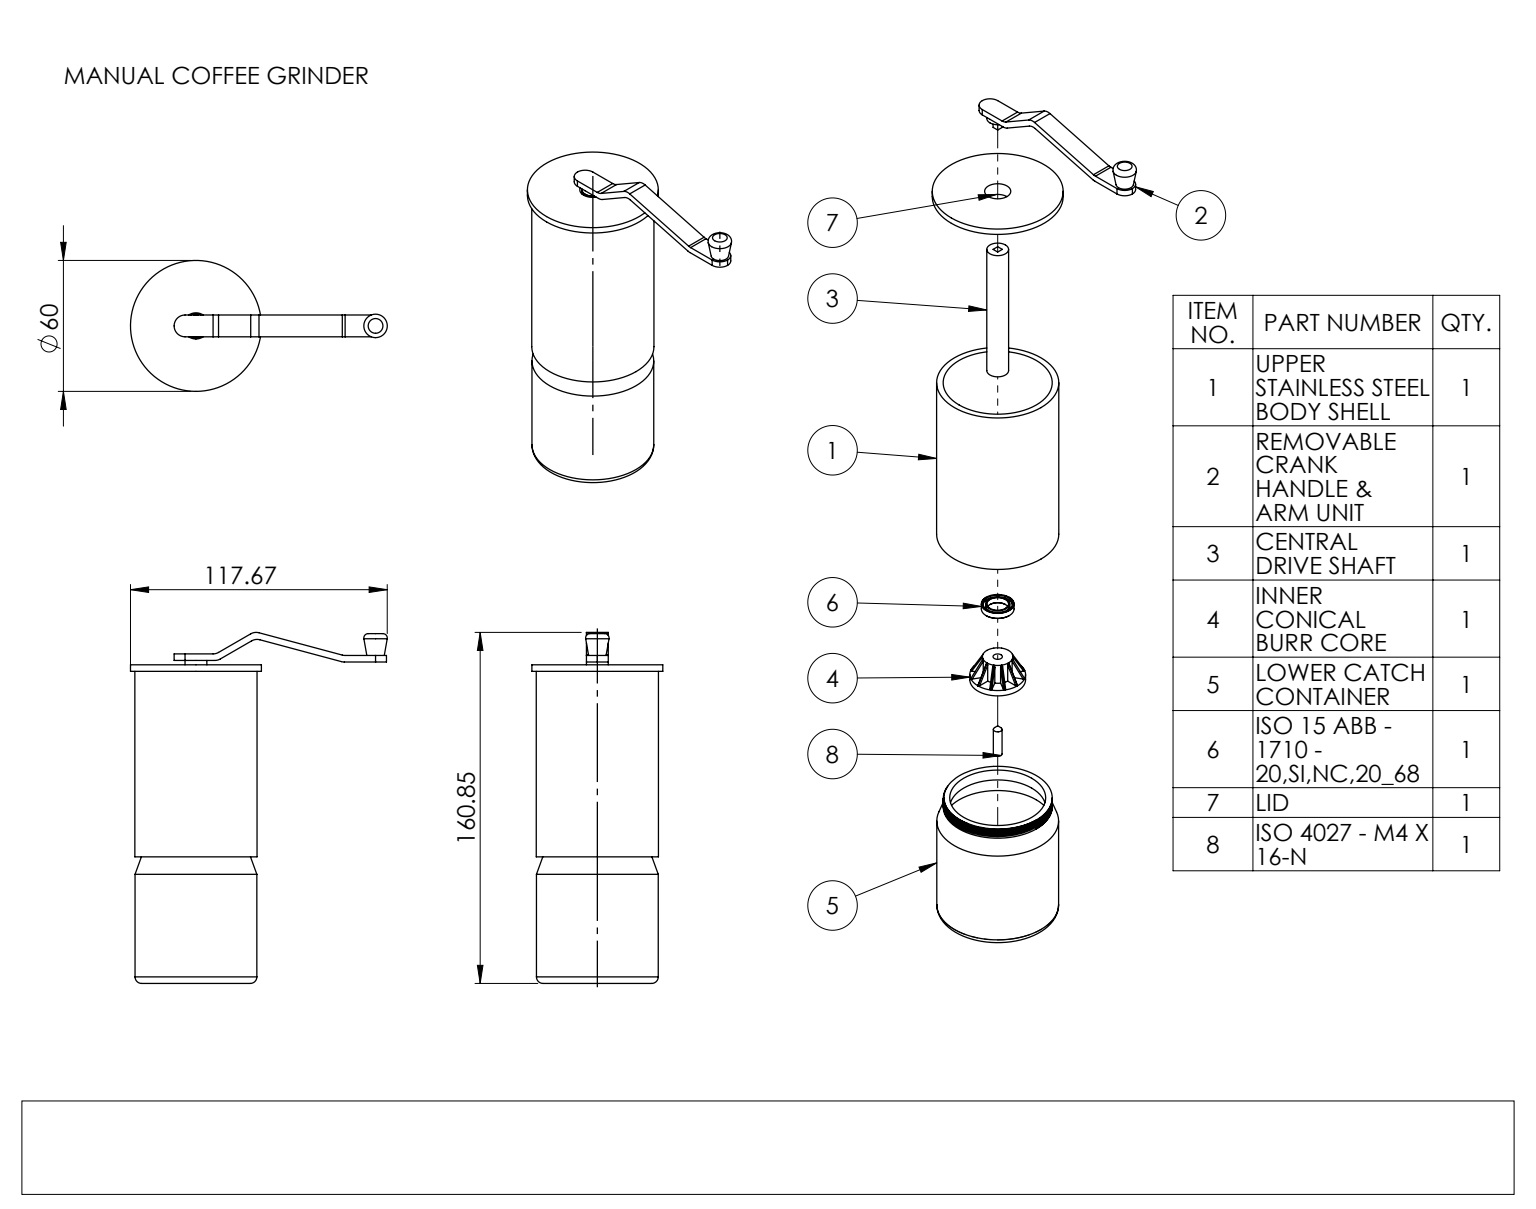
ISO-10303-21;
HEADER;
FILE_DESCRIPTION (('STEP AP214'),
    '1' );
FILE_NAME ('BR-816',
    '2026-10-04T07:23:31',
    ( '' ),
    ( '' ),
    'SwSTEP 2.0',
    'SolidWorks 2026',
    '' );
FILE_SCHEMA (( 'AUTOMOTIVE_DESIGN' ));
ENDSEC;

DATA;
#1 = ORIENTED_EDGE ( 'NONE', *, *, #1320, .F. ) ;
#2 = VERTEX_POINT ( 'NONE', #10191 ) ;
#3 = ORIENTED_EDGE ( 'NONE', *, *, #5333, .F. ) ;
#4 = ORIENTED_EDGE ( 'NONE', *, *, #9160, .T. ) ;
#5 = AXIS2_PLACEMENT_3D ( 'NONE', #6946, #2717, #1088 ) ;
#6 = DIRECTION ( 'NONE',  ( -0.000000000000000000, -1.000000000000000000, -0.000000000000000000 ) ) ;
#7 = CARTESIAN_POINT ( 'NONE',  ( -10.19839929293505776, 0.5312499990440845421, -24.62111388750000174 ) ) ;
#8 = VECTOR ( 'NONE', #4080, 1000.000000000000114 ) ;
#9 = CARTESIAN_POINT ( 'NONE',  ( 1.507608415688466075E-15, 0.6437499990440845865, -24.62111388750000174 ) ) ;
#10 = CARTESIAN_POINT ( 'NONE',  ( 1.530808498934191521E-15, 3.250000000000000444, -25.00000000000000000 ) ) ;
#11 = CARTESIAN_POINT ( 'NONE',  ( -18.60400172474273361, 25.00000000000000000, -7.276923788646512570 ) ) ;
#12 = CARTESIAN_POINT ( 'NONE',  ( 10.00000000000000000, 90.00000000000001421, -5.000000000000000000 ) ) ;
#13 = CARTESIAN_POINT ( 'NONE',  ( 6.296693311223917178, 19.03096903053430822, -3.058047309049999996 ) ) ;
#14 = PRODUCT_DEFINITION ( 'UNKNOWN', '', #3514, #8030 ) ;
#15 = CARTESIAN_POINT ( 'NONE',  ( 24.62111388749999463, 5.156249999044083765, 10.19839929293507730 ) ) ;
#16 = FACE_OUTER_BOUND ( 'NONE', #4981, .T. ) ;
#17 = EDGE_LOOP ( 'NONE', ( #5267, #4224, #10502 ) ) ;
#18 = ORIENTED_EDGE ( 'NONE', *, *, #6824, .T. ) ;
#19 = AXIS2_PLACEMENT_3D ( 'NONE', #2994, #5611, #7166 ) ;
#20 = VERTEX_POINT ( 'NONE', #2725 ) ;
#21 = DIRECTION ( 'NONE',  ( -0.000000000000000000, 1.000000000000000000, -0.000000000000000000 ) ) ;
#22 = EDGE_LOOP ( 'NONE', ( #2895, #8859 ) ) ;
#23 = FACE_OUTER_BOUND ( 'NONE', #10644, .T. ) ;
#24 = CIRCLE ( 'NONE', #8496, 7.500000000000000888 ) ;
#25 = DIRECTION ( 'NONE',  ( 0.000000000000000000, 0.000000000000000000, -1.000000000000000000 ) ) ;
#26 = EDGE_CURVE ( 'NONE', #5713, #6934, #4532, .T. ) ;
#27 = CARTESIAN_POINT ( 'NONE',  ( -1.399999999999998579, 1.126651916477733026E-15, 7.500000000000007994 ) ) ;
#28 = ADVANCED_FACE ( 'NONE', ( #7832 ), #3504, .F. ) ;
#29 =( BOUNDED_CURVE ( )  B_SPLINE_CURVE ( 2, ( #1490, #9059, #4872, #2466, #7337, #5796, #6516, #4977, #5693, #9821, #8329, #10667, #710, #4147, #8268, #1536, #6469, #7289, #10712, #8217, #9874, #10767, #4922, #6628, #4037, #7506, #659, #2414, #7388, #6572, #5852, #9934, #4089, #2367, #5744, #10884, #9103, #7444, #3285, #9986, #9157, #6688, #4816, #10043, #9208, #3929, #1653, #8998, #5036, #8384, #2255, #5638, #1426, #9505, #8609, #7675, #9449, #6799, #7559, #10941, #4194, #1937, #2745, #104, #163, #6090, #1057, #8554, #946, #4431, #10334, #6920, #2627, #4366, #9319, #6026, #8495, #6851, #10273, #882, #2520 ),
 .UNSPECIFIED., .F., .F. ) 
 B_SPLINE_CURVE_WITH_KNOTS ( ( 3, 2, 2, 2, 2, 2, 2, 2, 2, 2, 2, 2, 2, 2, 2, 2, 2, 2, 2, 2, 2, 2, 2, 2, 2, 2, 2, 2, 2, 2, 2, 2, 2, 2, 2, 2, 2, 2, 2, 2, 3 ),
 ( 0.000000000000000000, 0.02500000000000000139, 0.05000000000000000278, 0.07499999999999999722, 0.1000000000000000056, 0.1250000000000000000, 0.1499999999999999944, 0.1749999999999999889, 0.2000000000000000111, 0.2250000000000000056, 0.2500000000000000000, 0.2750000000000000222, 0.2999999999999999889, 0.3250000000000000111, 0.3499999999999999778, 0.3750000000000000000, 0.4000000000000000222, 0.4249999999999999889, 0.4500000000000000111, 0.4749999999999999778, 0.5000000000000000000, 0.5250000000000000222, 0.5500000000000000444, 0.5749999999999999556, 0.5999999999999999778, 0.6250000000000000000, 0.6500000000000000222, 0.6750000000000000444, 0.6999999999999999556, 0.7249999999999999778, 0.7500000000000000000, 0.7750000000000000222, 0.8000000000000000444, 0.8249999999999999556, 0.8499999999999999778, 0.8750000000000000000, 0.9000000000000000222, 0.9250000000000000444, 0.9499999999999999556, 0.9749999999999999778, 1.000000000000000000 ),
 .UNSPECIFIED. ) 
 CURVE ( )  GEOMETRIC_REPRESENTATION_ITEM ( )  RATIONAL_B_SPLINE_CURVE ( ( 1.000000000000000000, 0.9238795325112867385, 1.000000000000000000, 0.9238795325112867385, 1.000000000000000000, 0.9238795325112867385, 1.000000000000000000, 0.9238795325112867385, 1.000000000000000000, 0.9238795325112867385, 1.000000000000000000, 0.9238795325112867385, 1.000000000000000000, 0.9238795325112867385, 1.000000000000000000, 0.9238795325112867385, 1.000000000000000000, 0.9238795325112867385, 1.000000000000000000, 0.9238795325112867385, 1.000000000000000000, 0.9238795325112867385, 1.000000000000000000, 0.9238795325112867385, 1.000000000000000000, 0.9238795325112867385, 1.000000000000000000, 0.9238795325112867385, 1.000000000000000000, 0.9238795325112867385, 1.000000000000000000, 0.9238795325112867385, 1.000000000000000000, 0.9238795325112867385, 1.000000000000000000, 0.9238795325112867385, 1.000000000000000000, 0.9238795325112867385, 1.000000000000000000, 0.9238795325112867385, 1.000000000000000000, 0.9238795325112867385, 1.000000000000000000, 0.9238795325112867385, 1.000000000000000000, 0.9238795325112867385, 1.000000000000000000, 0.9238795325112867385, 1.000000000000000000, 0.9238795325112867385, 1.000000000000000000, 0.9238795325112867385, 1.000000000000000000, 0.9238795325112867385, 1.000000000000000000, 0.9238795325112867385, 1.000000000000000000, 0.9238795325112867385, 1.000000000000000000, 0.9238795325112867385, 1.000000000000000000, 0.9238795325112867385, 1.000000000000000000, 0.9238795325112867385, 1.000000000000000000, 0.9238795325112867385, 1.000000000000000000, 0.9238795325112867385, 1.000000000000000000, 0.9238795325112867385, 1.000000000000000000, 0.9238795325112867385, 1.000000000000000000, 0.9238795325112867385, 1.000000000000000000, 0.9238795325112867385, 1.000000000000000000, 0.9238795325112867385, 1.000000000000000000, 0.9238795325112867385, 1.000000000000000000 ) ) 
 REPRESENTATION_ITEM ( '' )  );
#30 = VECTOR ( 'NONE', #2527, 1000.000000000000000 ) ;
#31 = VECTOR ( 'NONE', #278, 1000.000000000000000 ) ;
#32 = ADVANCED_FACE ( 'NONE', ( #4472 ), #1742, .F. ) ;
#33 = ORIENTED_EDGE ( 'NONE', *, *, #3191, .T. ) ;
#34 = AXIS2_PLACEMENT_3D ( 'NONE', #3449, #3389, #7599 ) ;
#35 = DIRECTION ( 'NONE',  ( 0.000000000000000000, 0.000000000000000000, 1.000000000000000000 ) ) ;
#36 = FACE_OUTER_BOUND ( 'NONE', #8599, .T. ) ;
#37 = PLANE ( 'NONE',  #10541 ) ;
#38 = FACE_OUTER_BOUND ( 'NONE', #4930, .T. ) ;
#39 = VERTEX_POINT ( 'NONE', #260 ) ;
#40 = CIRCLE ( 'NONE', #9387, 2.999999999999999112 ) ;
#41 = LINE ( 'NONE', #2461, #2290 ) ;
#42 = AXIS2_PLACEMENT_3D ( 'NONE', #2337, #7419, #8866 ) ;
#43 = CARTESIAN_POINT ( 'NONE',  ( 0.2251666049839524120, 2.449293598294711838E-16, 2.000000000000004441 ) ) ;
#44 = DIRECTION ( 'NONE',  ( 0.000000000000000000, 0.000000000000000000, -1.000000000000000000 ) ) ;
#45 = EDGE_CURVE ( 'NONE', #4079, #9358, #1978, .T. ) ;
#46 = DIRECTION ( 'NONE',  ( -0.000000000000000000, -1.000000000000000000, -0.000000000000000000 ) ) ;
#47 = ORIENTED_EDGE ( 'NONE', *, *, #865, .T. ) ;
#48 = TOROIDAL_SURFACE ( 'NONE', #9050, 24.91176187412963117, 3.000000000000000000 ) ;
#49 = VECTOR ( 'NONE', #6901, 1000.000000000000000 ) ;
#50 = EDGE_CURVE ( 'NONE', #1424, #5838, #3619, .T. ) ;
#51 = CARTESIAN_POINT ( 'NONE',  ( -10.19839929293507552, 1.081249999044084475, 24.62111388749999463 ) ) ;
#52 = CARTESIAN_POINT ( 'NONE',  ( -10.19839929293505776, 1.706249999044084698, -24.62111388750000174 ) ) ;
#53 = LINE ( 'NONE', #1004, #7949 ) ;
#54 = VECTOR ( 'NONE', #4758, 1000.000000000000000 ) ;
#55 = CARTESIAN_POINT ( 'NONE',  ( 15.13990010960488952, -0.001000000000001000089, -5.276923788646758595 ) ) ;
#56 = CARTESIAN_POINT ( 'NONE',  ( 19.74999999999998934, -0.001000000000001000089, -3.000000000000067946 ) ) ;
#57 = VERTEX_POINT ( 'NONE', #5944 ) ;
#58 = CARTESIAN_POINT ( 'NONE',  ( -2.999999999999998224, 25.00000000000000000, -15.75000000000000355 ) ) ;
#59 = FILL_AREA_STYLE_COLOUR ( '', #6484 ) ;
#60 = CARTESIAN_POINT ( 'NONE',  ( -1.500000000000000444, 83.00000000000000000, -1.500000000000000222 ) ) ;
#61 = CARTESIAN_POINT ( 'NONE',  ( -4.592425496802574367E-15, 2.362499998088169129, 25.00000000000000000 ) ) ;
#62 = DIRECTION ( 'NONE',  ( 0.000000000000000000, 1.000000000000000000, 0.000000000000000000 ) ) ;
#63 = PLANE ( 'NONE',  #9863 ) ;
#64 = VECTOR ( 'NONE', #5356, 1000.000000000000000 ) ;
#65 = ORIENTED_EDGE ( 'NONE', *, *, #1287, .F. ) ;
#66 = EDGE_CURVE ( 'NONE', #3225, #5856, #203, .T. ) ;
#67 = ORIENTED_EDGE ( 'NONE', *, *, #4182, .T. ) ;
#68 = ORIENTED_EDGE ( 'NONE', *, *, #3846, .T. ) ;
#69 = VERTEX_POINT ( 'NONE', #5118 ) ;
#70 = UNCERTAINTY_MEASURE_WITH_UNIT (LENGTH_MEASURE( 1.000000000000000082E-05 ), #3920, 'distance_accuracy_value', 'NONE');
#71 = DIRECTION ( 'NONE',  ( -0.000000000000000000, -1.000000000000000000, -0.000000000000000000 ) ) ;
#72 = CARTESIAN_POINT ( 'NONE',  ( -10.19839929293507552, 0.9062499990440844311, 24.62111388749999463 ) ) ;
#73 = CARTESIAN_POINT ( 'NONE',  ( 7.347880794884120722E-16, 82.00000000000000000, -6.000000000000000888 ) ) ;
#74 = CARTESIAN_POINT ( 'NONE',  ( 24.62111388750000174, 2.393749999044084475, 0.000000000000000000 ) ) ;
#75 = CARTESIAN_POINT ( 'NONE',  ( -25.00000000000000000, 0.4375000000000000000, -10.35533905932738108 ) ) ;
#76 = CARTESIAN_POINT ( 'NONE',  ( 17.10400172474269098, 28.00000000000000000, 9.874999999999957367 ) ) ;
#77 = ORIENTED_EDGE ( 'NONE', *, *, #7857, .F. ) ;
#78 = CARTESIAN_POINT ( 'NONE',  ( 3.785909150703048454, 19.34316356887877220, -5.890223162633865250 ) ) ;
#79 = CARTESIAN_POINT ( 'NONE',  ( 0.000000000000000000, 5.000000000000000000, 0.000000000000000000 ) ) ;
#80 = CARTESIAN_POINT ( 'NONE',  ( -17.67766952966369232, 0.6250000000000000000, 17.67766952966368876 ) ) ;
#81 = CARTESIAN_POINT ( 'NONE',  ( -25.00000000000000000, 3.112499998088169129, -3.061616997868383043E-15 ) ) ;
#82 = ORIENTED_EDGE ( 'NONE', *, *, #3385, .T. ) ;
#83 = ORIENTED_EDGE ( 'NONE', *, *, #9025, .F. ) ;
#84 = ORIENTED_EDGE ( 'NONE', *, *, #2390, .T. ) ;
#85 = PRODUCT_DEFINITION_SHAPE ( 'NONE', 'NONE',  #10954 ) ;
#86 = DIRECTION ( 'NONE',  ( -0.000000000000000000, 1.000000000000000000, 0.000000000000000000 ) ) ;
#87 = FACE_OUTER_BOUND ( 'NONE', #4011, .T. ) ;
#88 = FACE_OUTER_BOUND ( 'NONE', #5727, .T. ) ;
#89 = CARTESIAN_POINT ( 'NONE',  ( 6.999999999999997335, 19.66631150450990617, 0.1668442477450632899 ) ) ;
#90 = FACE_OUTER_BOUND ( 'NONE', #9620, .T. ) ;
#91 = CARTESIAN_POINT ( 'NONE',  ( 1.040834085586084257E-14, 88.00000000000001421, -4.999999999999987566 ) ) ;
#92 = CARTESIAN_POINT ( 'NONE',  ( 12.47307621135333200, 25.00000000000000000, 15.60400172474264835 ) ) ;
#93 = VERTEX_POINT ( 'NONE', #1861 ) ;
#94 = EDGE_CURVE ( 'NONE', #2407, #2818, #6149, .T. ) ;
#95 = DIRECTION ( 'NONE',  ( -0.000000000000000000, -1.000000000000000000, -0.000000000000000000 ) ) ;
#96 = SURFACE_SIDE_STYLE ('',( #6842 ) ) ;
#97 = CARTESIAN_POINT ( 'NONE',  ( 24.99999999999999289, 5.549999998088169129, 10.35533905932739529 ) ) ;
#98 = CARTESIAN_POINT ( 'NONE',  ( 24.62111388750000174, 0.4562499990440845310, -10.19839929293505776 ) ) ;
#99 = ORIENTED_EDGE ( 'NONE', *, *, #3561, .F. ) ;
#100 = LINE ( 'NONE', #5208, #8824 ) ;
#101 = CARTESIAN_POINT ( 'NONE',  ( 17.10400172474269098, 28.00000000000000000, 9.874999999999957367 ) ) ;
#102 = ORIENTED_EDGE ( 'NONE', *, *, #949, .F. ) ;
#103 = CARTESIAN_POINT ( 'NONE',  ( 19.74999999999998934, 25.00000000000000000, -3.000000000000067946 ) ) ;
#104 = CARTESIAN_POINT ( 'NONE',  ( 24.62111388749999108, 4.156249999044084653, 10.19839929293507730 ) ) ;
#105 = ADVANCED_FACE ( 'NONE', ( #143 ), #1537, .T. ) ;
#106 = EDGE_CURVE ( 'NONE', #5745, #5240, #6492, .T. ) ;
#107 = CARTESIAN_POINT ( 'NONE',  ( -4.522825247065398226E-15, 3.143749999044084475, 24.62111388750000174 ) ) ;
#108 = DIRECTION ( 'NONE',  ( 0.000000000000000000, -2.775557561562888270E-17, -1.000000000000000000 ) ) ;
#109 = CARTESIAN_POINT ( 'NONE',  ( -20.63749999999999929, 0.000000000000000000, 0.000000000000000000 ) ) ;
#110 = DIRECTION ( 'NONE',  ( 0.000000000000000000, 0.000000000000000000, 1.000000000000000000 ) ) ;
#111 = ORIENTED_EDGE ( 'NONE', *, *, #6802, .F. ) ;
#112 = CARTESIAN_POINT ( 'NONE',  ( 3.061616997868383043E-15, 27.99999999999999645, 25.00000000000000000 ) ) ;
#113 =( NAMED_UNIT ( * ) SI_UNIT ( $, .STERADIAN. ) SOLID_ANGLE_UNIT ( ) );
#114 = DIRECTION ( 'NONE',  ( 1.000000000000000000, 0.000000000000000000, -0.000000000000000000 ) ) ;
#115 = CARTESIAN_POINT ( 'NONE',  ( 0.000000000000000000, 20.00000000000000355, 0.000000000000000000 ) ) ;
#116 = CARTESIAN_POINT ( 'NONE',  ( -25.00000000000000000, 2.112499998088169129, -3.061616997868383043E-15 ) ) ;
#117 = CARTESIAN_POINT ( 'NONE',  ( 2.449293598294706513E-15, 20.00000000000000355, -20.00000000000000000 ) ) ;
#118 = CARTESIAN_POINT ( 'NONE',  ( 17.67766952966368521, 2.875000000000000000, 17.67766952966369232 ) ) ;
#119 = EDGE_CURVE ( 'NONE', #6443, #1427, #3381, .T. ) ;
#120 = VERTEX_POINT ( 'NONE', #1095 ) ;
#121 = ORIENTED_EDGE ( 'NONE', *, *, #10240, .T. ) ;
#122 = VERTEX_POINT ( 'NONE', #5243 ) ;
#123 = ORIENTED_EDGE ( 'NONE', *, *, #7539, .F. ) ;
#124 = CARTESIAN_POINT ( 'NONE',  ( 0.000000000000000000, 85.00000000000000000, 0.000000000000000000 ) ) ;
#125 = CARTESIAN_POINT ( 'NONE',  ( -10.19839929293507552, 5.081249999044084475, 24.62111388749999463 ) ) ;
#126 = CARTESIAN_POINT ( 'NONE',  ( 17.67766952966369232, 0.7374999980881691286, -17.67766952966369232 ) ) ;
#127 = CARTESIAN_POINT ( 'NONE',  ( 10.19839929293506486, 1.206249999044084698, 24.62111388749999819 ) ) ;
#128 = CARTESIAN_POINT ( 'NONE',  ( -24.62111388750000884, 3.781249999044084653, 10.19839929293505421 ) ) ;
#129 = CARTESIAN_POINT ( 'NONE',  ( -25.00000000000001066, 3.174999998088169573, 10.35533905932737397 ) ) ;
#130 = EDGE_CURVE ( 'NONE', #7410, #4070, #2608, .T. ) ;
#131 = ORIENTED_EDGE ( 'NONE', *, *, #4600, .T. ) ;
#132 = LINE ( 'NONE', #3493, #145 ) ;
#133 = FACE_BOUND ( 'NONE', #4065, .T. ) ;
#134 = DIRECTION ( 'NONE',  ( 0.000000000000000000, 0.000000000000000000, -1.000000000000000000 ) ) ;
#135 = CARTESIAN_POINT ( 'NONE',  ( -25.00000000000000000, 0.4375000000000000000, -10.35533905932738108 ) ) ;
#136 = CARTESIAN_POINT ( 'NONE',  ( -7.211537444790369733, 10.00000000000000355, -6.776463540776874517 ) ) ;
#137 = EDGE_LOOP ( 'NONE', ( #3283, #4277, #3194, #1557 ) ) ;
#138 = CLOSED_SHELL ( 'NONE', ( #5912, #7027, #10918, #9263, #5268, #8033, #4039, #8931, #9209, #7081, #6514, #516, #6002, #10646, #9653, #6197, #4591, #507, #1397, #6646, #1299, #2039, #10092, #4594, #8749, #861, #6693, #7676, #7148, #10570, #5853, #5516, #7088, #717, #5052, #4023, #6869, #3689, #10249, #2799, #5302, #2691, #9344, #9035, #8964, #1267, #437, #3259, #9811, #1259, #7773, #2191, #3472, #3885, #1656, #6813, #3576, #3914, #8252, #9299, #6399, #2209, #4947, #674, #661, #4449, #10399, #4818, #868, #5935, #9573, #7951, #2937, #7004, #2676, #5317, #5105, #3750, #6202, #28, #5672, #1968, #3916, #4465, #4519, #8455, #4226, #4367, #4978, #6266, #8625, #8205, #7818, #6087, #10928, #4909, #2609 ) ) ;
#139 =( BOUNDED_CURVE ( )  B_SPLINE_CURVE ( 2, ( #7817, #6880, #1965, #10238, #251, #129, #4337, #7756, #2653 ),
 .UNSPECIFIED., .F., .F. ) 
 B_SPLINE_CURVE_WITH_KNOTS ( ( 3, 2, 2, 2, 3 ),
 ( 0.4500000000000000111, 0.4749999999999999778, 0.5000000000000000000, 0.5250000000000000222, 0.5500000000000000444 ),
 .UNSPECIFIED. ) 
 CURVE ( )  GEOMETRIC_REPRESENTATION_ITEM ( )  RATIONAL_B_SPLINE_CURVE ( ( 1.000000000000000000, 0.9238795325112867385, 1.000000000000000000, 0.9238795325112867385, 1.000000000000000000, 0.9238795325112867385, 1.000000000000000000, 0.9238795325112867385, 1.000000000000000000 ) ) 
 REPRESENTATION_ITEM ( '' )  );
#140 = ORIENTED_EDGE ( 'NONE', *, *, #5576, .T. ) ;
#141 = ORIENTED_EDGE ( 'NONE', *, *, #3333, .T. ) ;
#142 = ORIENTED_EDGE ( 'NONE', *, *, #10441, .F. ) ;
#143 = FACE_OUTER_BOUND ( 'NONE', #4066, .T. ) ;
#144 = ADVANCED_FACE ( 'NONE', ( #9538 ), #8711, .T. ) ;
#145 = VECTOR ( 'NONE', #2655, 1000.000000000000000 ) ;
#146 = DIRECTION ( 'NONE',  ( -0.000000000000000000, -1.000000000000000000, -0.000000000000000000 ) ) ;
#147 = CARTESIAN_POINT ( 'NONE',  ( -17.10400172474254532, 28.00000000000000000, 9.875000000000202505 ) ) ;
#148 = DIRECTION ( 'NONE',  ( 1.000000000000000000, 0.000000000000000000, 0.000000000000000000 ) ) ;
#149 = FACE_OUTER_BOUND ( 'NONE', #10908, .T. ) ;
#150 = CYLINDRICAL_SURFACE ( 'NONE', #10591, 4.500000000000000888 ) ;
#151 = DIRECTION ( 'NONE',  ( -0.8838834764831844382, -0.3535533905932726206, 0.3061862178478983454 ) ) ;
#152 = CARTESIAN_POINT ( 'NONE',  ( -24.62111388750000174, 3.893749999044084475, -3.015216831376932151E-15 ) ) ;
#153 = AXIS2_PLACEMENT_3D ( 'NONE', #2387, #10130, #10796 ) ;
#154 = CIRCLE ( 'NONE', #1379, 12.77350269189627063 ) ;
#155 = ORIENTED_EDGE ( 'NONE', *, *, #4589, .F. ) ;
#156 = CARTESIAN_POINT ( 'NONE',  ( 24.99999999999999289, 4.937500000000000888, 10.35533905932739529 ) ) ;
#157 = CARTESIAN_POINT ( 'NONE',  ( 17.67766952966368521, 5.487499998088169129, 17.67766952966369232 ) ) ;
#158 = CARTESIAN_POINT ( 'NONE',  ( -24.62111388750000174, 4.831249999044084475, -10.19839929293506131 ) ) ;
#159 = CARTESIAN_POINT ( 'NONE',  ( -6.062177826491028654, 20.00000000000000355, -3.500000000000069722 ) ) ;
#160 = CONTEXT_DEPENDENT_SHAPE_REPRESENTATION ( #10845, #7160 ) ;
#161 = CARTESIAN_POINT ( 'NONE',  ( 0.000000000000000000, 85.00000000000000000, 0.000000000000000000 ) ) ;
#162 = CARTESIAN_POINT ( 'NONE',  ( -3.066987298107830995, 10.00000000000000355, 6.312177826491043753 ) ) ;
#163 = CARTESIAN_POINT ( 'NONE',  ( 24.62111388750000174, 4.218749999044084653, 0.000000000000000000 ) ) ;
#164 = CARTESIAN_POINT ( 'NONE',  ( -10.19839929293505776, 0.7062499990440844755, -24.62111388750000174 ) ) ;
#165 = CARTESIAN_POINT ( 'NONE',  ( 4.500000000000000888, 10.10000000000000497, 0.000000000000000000 ) ) ;
#166 = CARTESIAN_POINT ( 'NONE',  ( -25.00000000000000000, 1.049999998088169129, -10.35533905932738108 ) ) ;
#167 = DIRECTION ( 'NONE',  ( 0.000000000000000000, 2.775557561562888270E-17, 1.000000000000000000 ) ) ;
#168 = ORIENTED_EDGE ( 'NONE', *, *, #8555, .T. ) ;
#169 = DIRECTION ( 'NONE',  ( -0.000000000000000000, 1.000000000000000000, 0.000000000000000000 ) ) ;
#170 = CARTESIAN_POINT ( 'NONE',  ( -17.10400172474254532, 28.00000000000000000, 9.875000000000202505 ) ) ;
#171 =( LENGTH_UNIT ( ) NAMED_UNIT ( * ) SI_UNIT ( .MILLI., .METRE. ) );
#172 = CARTESIAN_POINT ( 'NONE',  ( 10.19839929293505953, 0.4062499990440845421, -24.62111388750000174 ) ) ;
#173 = CARTESIAN_POINT ( 'NONE',  ( 2.632990618166809235E-16, 7.000000000000003553, 2.149999999999999911 ) ) ;
#174 = DIRECTION ( 'NONE',  ( 0.000000000000000000, 0.000000000000000000, 1.000000000000000000 ) ) ;
#175 = CARTESIAN_POINT ( 'NONE',  ( -25.00000000000001421, 3.562500000000000444, 10.35533905932737397 ) ) ;
#176 = PRODUCT_DEFINITION_SHAPE ( 'NONE', 'NONE',  #10948 ) ;
#177 = ADVANCED_FACE ( 'NONE', ( #4290 ), #10361, .F. ) ;
#178 = AXIS2_PLACEMENT_3D ( 'NONE', #3237, #7515, #1602 ) ;
#179 = EDGE_LOOP ( 'NONE', ( #3319, #1358, #7705, #7107 ) ) ;
#180 = CIRCLE ( 'NONE', #5817, 7.500000000000007994 ) ;
#181 = ORIENTED_EDGE ( 'NONE', *, *, #2071, .F. ) ;
#182 = EDGE_CURVE ( 'NONE', #2588, #10522, #9482, .T. ) ;
#183 = LINE ( 'NONE', #1845, #502 ) ;
#184 = CARTESIAN_POINT ( 'NONE',  ( 24.62111388749999463, 4.331249999044085364, 10.19839929293507730 ) ) ;
#185 = DIRECTION ( 'NONE',  ( 0.000000000000000000, -1.000000000000000000, 0.000000000000000000 ) ) ;
#186 = CARTESIAN_POINT ( 'NONE',  ( -10.35533905932737575, 3.924999998088169129, -25.00000000000000000 ) ) ;
#187 = CARTESIAN_POINT ( 'NONE',  ( -17.40975659021752975, 3.593749999044084653, -17.40975659021752975 ) ) ;
#188 = FACE_OUTER_BOUND ( 'NONE', #7003, .T. ) ;
#189 = AXIS2_PLACEMENT_3D ( 'NONE', #10549, #390, #1123 ) ;
#190 = VECTOR ( 'NONE', #6922, 1000.000000000000000 ) ;
#191 = DIRECTION ( 'NONE',  ( 1.000000000000000000, 0.000000000000000000, 0.000000000000000000 ) ) ;
#192 = PLANE ( 'NONE',  #1400 ) ;
#193 = DIRECTION ( 'NONE',  ( 0.000000000000000000, 0.000000000000000000, -1.000000000000000000 ) ) ;
#194 = FACE_OUTER_BOUND ( 'NONE', #6105, .T. ) ;
#195 = CARTESIAN_POINT ( 'NONE',  ( -10.35533905932737575, 1.312500000000000444, -25.00000000000000000 ) ) ;
#196 = EDGE_CURVE ( 'NONE', #620, #978, #10271, .T. ) ;
#197 = CARTESIAN_POINT ( 'NONE',  ( -17.67766952966369232, 3.237499998088169573, 17.67766952966368876 ) ) ;
#198 = ORIENTED_EDGE ( 'NONE', *, *, #7378, .T. ) ;
#199 = ORIENTED_EDGE ( 'NONE', *, *, #10771, .T. ) ;
#200 = ORIENTED_EDGE ( 'NONE', *, *, #382, .F. ) ;
#201 = AXIS2_PLACEMENT_3D ( 'NONE', #9799, #474, #7991 ) ;
#202 = PRESENTATION_LAYER_ASSIGNMENT (  '', '', ( #540 ) ) ;
#203 = LINE ( 'NONE', #6782, #2239 ) ;
#204 = EDGE_CURVE ( 'NONE', #10138, #4764, #1958, .T. ) ;
#205 = DIRECTION ( 'NONE',  ( -0.000000000000000000, 1.000000000000000000, -0.000000000000000000 ) ) ;
#206 = EDGE_LOOP ( 'NONE', ( #9870, #5506, #9937, #2232 ) ) ;
#207 = CYLINDRICAL_SURFACE ( 'NONE', #8878, 5.750000000000006217 ) ;
#208 = CARTESIAN_POINT ( 'NONE',  ( -3.223142256880076948E-15, 28.00000000000000000, -15.75000000000000000 ) ) ;
#209 = DIRECTION ( 'NONE',  ( 0.000000000000000000, 0.000000000000000000, 1.000000000000000000 ) ) ;
#210 = CARTESIAN_POINT ( 'NONE',  ( 7.874999999999916511, 28.00000000000000000, -10.63990010960495702 ) ) ;
#211 = CARTESIAN_POINT ( 'NONE',  ( 1.530808498934191521E-15, 1.250000000000000000, -25.00000000000000000 ) ) ;
#212 = AXIS2_PLACEMENT_3D ( 'NONE', #8810, #4790, #575 ) ;
#213 = ORIENTED_EDGE ( 'NONE', *, *, #10024, .F. ) ;
#214 = ORIENTED_EDGE ( 'NONE', *, *, #10048, .F. ) ;
#215 = DIRECTION ( 'NONE',  ( 0.000000000000000000, 0.000000000000000000, 1.000000000000000000 ) ) ;
#216 = CARTESIAN_POINT ( 'NONE',  ( -10.35533905932739174, 4.299999998088169129, 24.99999999999999289 ) ) ;
#217 = CIRCLE ( 'NONE', #6933, 25.00000000000000000 ) ;
#218 = CARTESIAN_POINT ( 'NONE',  ( 17.40975659021752975, 4.518749999044084475, -17.40975659021752975 ) ) ;
#219 = EDGE_LOOP ( 'NONE', ( #2618, #7161, #8269, #2550 ) ) ;
#220 = CARTESIAN_POINT ( 'NONE',  ( 3.061616997868383043E-15, 0.000000000000000000, 25.00000000000000000 ) ) ;
#221 = CARTESIAN_POINT ( 'NONE',  ( 0.000000000000000000, 7.000000000000003553, 0.000000000000000000 ) ) ;
#222 = DIRECTION ( 'NONE',  ( 0.000000000000000000, 1.000000000000000000, 0.000000000000000000 ) ) ;
#223 = CARTESIAN_POINT ( 'NONE',  ( 0.000000000000000000, 25.00000000000000355, -2.000000000000000000 ) ) ;
#224 = VECTOR ( 'NONE', #10052, 1000.000000000000000 ) ;
#225 = AXIS2_PLACEMENT_3D ( 'NONE', #3856, #484, #9861 ) ;
#226 = ORIENTED_EDGE ( 'NONE', *, *, #6126, .T. ) ;
#227 = CIRCLE ( 'NONE', #6760, 2.000000000000000000 ) ;
#228 = CARTESIAN_POINT ( 'NONE',  ( -24.62111388750000174, 1.831249999044084475, -10.19839929293506131 ) ) ;
#229 = VECTOR ( 'NONE', #2900, 1000.000000000000000 ) ;
#230 = CARTESIAN_POINT ( 'NONE',  ( 24.99999999999999289, 1.937500000000000000, 10.35533905932739529 ) ) ;
#231 = CARTESIAN_POINT ( 'NONE',  ( -4.522825247065398226E-15, 4.968749999044083765, 24.62111388750000174 ) ) ;
#232 = PLANE ( 'NONE',  #3563 ) ;
#233 = ORIENTED_EDGE ( 'NONE', *, *, #10324, .F. ) ;
#234 = CARTESIAN_POINT ( 'NONE',  ( 1.530808498934191521E-15, 0.8624999980881691286, -25.00000000000000000 ) ) ;
#235 = CARTESIAN_POINT ( 'NONE',  ( -17.67766952966368876, 2.375000000000000000, -17.67766952966369232 ) ) ;
#236 = VECTOR ( 'NONE', #2762, 1000.000000000000000 ) ;
#237 = CARTESIAN_POINT ( 'NONE',  ( -24.62111388750000174, 0.6562499990440845421, -10.19839929293506131 ) ) ;
#238 = DIRECTION ( 'NONE',  ( -0.000000000000000000, 1.000000000000000000, -0.000000000000000000 ) ) ;
#239 = VECTOR ( 'NONE', #5384, 1000.000000000000000 ) ;
#240 = AXIS2_PLACEMENT_3D ( 'NONE', #1921, #5301, #7838 ) ;
#241 = VERTEX_POINT ( 'NONE', #8761 ) ;
#242 = ORIENTED_EDGE ( 'NONE', *, *, #1929, .F. ) ;
#243 = CIRCLE ( 'NONE', #1136, 3.379762621896238883 ) ;
#244 = DIRECTION ( 'NONE',  ( 0.000000000000000000, 1.000000000000000000, 0.000000000000000000 ) ) ;
#245 = CARTESIAN_POINT ( 'NONE',  ( 17.40975659021752975, 3.518749999044084920, -17.40975659021752975 ) ) ;
#246 = LINE ( 'NONE', #73, #236 ) ;
#247 = EDGE_CURVE ( 'NONE', #3577, #5793, #9294, .T. ) ;
#248 = CARTESIAN_POINT ( 'NONE',  ( -25.00000000000001421, 3.174999998088169129, 10.35533905932737397 ) ) ;
#249 = CARTESIAN_POINT ( 'NONE',  ( -24.62111388750000174, 2.656249999044085097, -10.19839929293506131 ) ) ;
#250 = EDGE_CURVE ( 'NONE', #1860, #1446, #9645, .T. ) ;
#251 = CARTESIAN_POINT ( 'NONE',  ( -25.00000000000000000, 3.112499998088169129, -3.061616997868383043E-15 ) ) ;
#252 = CYLINDRICAL_SURFACE ( 'NONE', #1418, 25.00000000000000000 ) ;
#253 = AXIS2_PLACEMENT_3D ( 'NONE', #6290, #1159, #5410 ) ;
#254 = CARTESIAN_POINT ( 'NONE',  ( -25.00000000000000000, 1.437500000000000000, -10.35533905932738108 ) ) ;
#255 = CARTESIAN_POINT ( 'NONE',  ( -13.63990010960498367, 28.00000000000000000, -4.874999999999871214 ) ) ;
#256 = EDGE_CURVE ( 'NONE', #8849, #3847, #4015, .T. ) ;
#257 = VERTEX_POINT ( 'NONE', #2223 ) ;
#258 = VECTOR ( 'NONE', #8917, 1000.000000000000114 ) ;
#259 = ORIENTED_EDGE ( 'NONE', *, *, #4096, .F. ) ;
#260 = CARTESIAN_POINT ( 'NONE',  ( 1.530808498934191521E-15, 0.8624999980881691286, -25.00000000000000000 ) ) ;
#261 = EDGE_CURVE ( 'NONE', #5968, #10806, #9690, .T. ) ;
#262 = FACE_OUTER_BOUND ( 'NONE', #1288, .T. ) ;
#263 = DIRECTION ( 'NONE',  ( 0.6546536707079723127, -0.000000000000000000, -0.7559289460184587250 ) ) ;
#264 = DIRECTION ( 'NONE',  ( 0.000000000000000000, 0.000000000000000000, 1.000000000000000000 ) ) ;
#265 = CARTESIAN_POINT ( 'NONE',  ( -1.500000000000000444, 88.00000000000001421, -1.500000000000000222 ) ) ;
#266 = DIRECTION ( 'NONE',  ( 0.000000000000000000, 0.000000000000000000, -1.000000000000000000 ) ) ;
#267 = DIRECTION ( 'NONE',  ( 0.000000000000000000, 0.000000000000000000, -1.000000000000000000 ) ) ;
#268 = EDGE_CURVE ( 'NONE', #2208, #3766, #1396, .T. ) ;
#269 = CARTESIAN_POINT ( 'NONE',  ( -17.40975659021752975, 3.768749999044084475, -17.40975659021752975 ) ) ;
#270 = EDGE_LOOP ( 'NONE', ( #6260, #9302, #1877, #7015, #4822 ) ) ;
#271 = ORIENTED_EDGE ( 'NONE', *, *, #10865, .F. ) ;
#272 = PRODUCT_DEFINITION_SHAPE ( 'NONE', 'NONE',  #10950 ) ;
#273 = CARTESIAN_POINT ( 'NONE',  ( 24.99999999999999289, 2.937500000000000000, 10.35533905932739529 ) ) ;
#274 = CARTESIAN_POINT ( 'NONE',  ( 10.35533905932738286, 1.424999998088169129, 24.99999999999999645 ) ) ;
#275 = CARTESIAN_POINT ( 'NONE',  ( 17.40975659021752975, 3.518749999044084920, -17.40975659021752975 ) ) ;
#276 =( BOUNDED_CURVE ( )  B_SPLINE_CURVE ( 3, ( #9723, #2251, #5583, #2149 ),
 .UNSPECIFIED., .F., .F. ) 
 B_SPLINE_CURVE_WITH_KNOTS ( ( 4, 4 ),
 ( 2.284520705739658375, 2.356010155625179792 ),
 .UNSPECIFIED. ) 
 CURVE ( )  GEOMETRIC_REPRESENTATION_ITEM ( )  RATIONAL_B_SPLINE_CURVE ( ( 1.000000000000000000, 0.9995741502243209453, 0.9995741502243209453, 1.000000000000000000 ) ) 
 REPRESENTATION_ITEM ( '' )  );
#277 = DIRECTION ( 'NONE',  ( -0.2500000000000041078, -0.8660254037844380415, 0.4330127018922181881 ) ) ;
#278 = DIRECTION ( 'NONE',  ( -0.000000000000000000, 1.000000000000000000, -0.000000000000000000 ) ) ;
#279 = ADVANCED_FACE ( 'NONE', ( #7206 ), #1724, .T. ) ;
#280 = DIRECTION ( 'NONE',  ( -0.000000000000000000, 1.000000000000000000, -0.000000000000000000 ) ) ;
#281 = CARTESIAN_POINT ( 'NONE',  ( -0.5000000000000001110, 10.00000000000000355, -6.982120021884469452 ) ) ;
#282 = CARTESIAN_POINT ( 'NONE',  ( 10.19839929293506486, 5.206249999044084475, 24.62111388749999819 ) ) ;
#283 = DIRECTION ( 'NONE',  ( 0.000000000000000000, 0.000000000000000000, 1.000000000000000000 ) ) ;
#284 = CARTESIAN_POINT ( 'NONE',  ( 10.35533905932737930, 3.187500000000000444, -25.00000000000000000 ) ) ;
#285 = CARTESIAN_POINT ( 'NONE',  ( -10.19839929293505776, 0.7062499990440845865, -24.62111388750000174 ) ) ;
#286 = ORIENTED_EDGE ( 'NONE', *, *, #9789, .F. ) ;
#287 = PLANE ( 'NONE',  #10755 ) ;
#288 = CARTESIAN_POINT ( 'NONE',  ( 1.530808498934191521E-15, 2.250000000000000444, -25.00000000000000000 ) ) ;
#289 = CARTESIAN_POINT ( 'NONE',  ( -17.40975659021753330, 0.8437499990440846531, 17.40975659021752975 ) ) ;
#290 = CARTESIAN_POINT ( 'NONE',  ( -10.35533905932739174, 1.299999998088169129, 24.99999999999999289 ) ) ;
#291 = ORIENTED_EDGE ( 'NONE', *, *, #10657, .F. ) ;
#292 = VERTEX_POINT ( 'NONE', #5447 ) ;
#293 = CARTESIAN_POINT ( 'NONE',  ( -24.62111388750000884, 1.956249999044084475, 10.19839929293505421 ) ) ;
#294 = ORIENTED_EDGE ( 'NONE', *, *, #5471, .F. ) ;
#295 = CARTESIAN_POINT ( 'NONE',  ( 2.500000000000000444, -1.000000000000003109, -0.5773502691896260641 ) ) ;
#296 = CARTESIAN_POINT ( 'NONE',  ( -24.62111388750000174, 3.718749999044084653, -3.015216831376932151E-15 ) ) ;
#297 = DIRECTION ( 'NONE',  ( -2.168404344971010347E-16, 0.000000000000000000, -1.000000000000000000 ) ) ;
#298 = CARTESIAN_POINT ( 'NONE',  ( 10.35533905932737930, 2.799999998088169573, -25.00000000000000000 ) ) ;
#299 = CARTESIAN_POINT ( 'NONE',  ( 24.62111388749999463, 4.156249999044083765, 10.19839929293507730 ) ) ;
#300 = CYLINDRICAL_SURFACE ( 'NONE', #10201, 2.999999999999997335 ) ;
#301 = CARTESIAN_POINT ( 'NONE',  ( -5.978755702618581580, 19.66631150450990617, 3.644491357022453748 ) ) ;
#302 = CARTESIAN_POINT ( 'NONE',  ( 0.2500000000000019984, 0.000000000000000000, -0.4330127018922181326 ) ) ;
#303 = CARTESIAN_POINT ( 'NONE',  ( -25.00000000000001421, 4.562500000000000888, 10.35533905932737397 ) ) ;
#304 = CARTESIAN_POINT ( 'NONE',  ( -15.75000000000000000, 25.00000000000000000, 1.681956355172181189E-13 ) ) ;
#305 = ORIENTED_EDGE ( 'NONE', *, *, #6800, .T. ) ;
#306 = ORIENTED_EDGE ( 'NONE', *, *, #2066, .F. ) ;
#307 = EDGE_CURVE ( 'NONE', #620, #1515, #1911, .T. ) ;
#308 = DIRECTION ( 'NONE',  ( 0.000000000000000000, 1.000000000000000000, 0.000000000000000000 ) ) ;
#309 = ADVANCED_FACE ( 'NONE', ( #3677 ), #6334, .F. ) ;
#310 =( GEOMETRIC_REPRESENTATION_CONTEXT ( 3 ) GLOBAL_UNCERTAINTY_ASSIGNED_CONTEXT ( ( #8038 ) ) GLOBAL_UNIT_ASSIGNED_CONTEXT ( ( #3651, #958, #5094 ) ) REPRESENTATION_CONTEXT ( 'NONE', 'WORKASPACE' ) );
#311 = LINE ( 'NONE', #7774, #4484 ) ;
#312 = CARTESIAN_POINT ( 'NONE',  ( 11.42163336986832611, 7.781088913245561400, -7.171633369868279928 ) ) ;
#313 = CARTESIAN_POINT ( 'NONE',  ( 0.000000000000000000, 0.000000000000000000, 0.000000000000000000 ) ) ;
#314 = CARTESIAN_POINT ( 'NONE',  ( -5.000000000000000000, 90.00000000000001421, 0.000000000000000000 ) ) ;
#315 = CYLINDRICAL_SURFACE ( 'NONE', #5866, 2.999999999999997335 ) ;
#316 = CARTESIAN_POINT ( 'NONE',  ( 17.40975659021752975, 3.518749999044084920, -17.40975659021752975 ) ) ;
#317 = EDGE_CURVE ( 'NONE', #3676, #8924, #362, .T. ) ;
#318 = EDGE_CURVE ( 'NONE', #10892, #10861, #6286, .T. ) ;
#319 = EDGE_CURVE ( 'NONE', #5890, #7487, #2988, .T. ) ;
#320 = AXIS2_PLACEMENT_3D ( 'NONE', #10601, #7911, #7226 ) ;
#321 = ORIENTED_EDGE ( 'NONE', *, *, #1197, .F. ) ;
#322 = CLOSED_SHELL ( 'NONE', ( #1450, #3684, #7028, #7525, #4651, #6943, #8474, #5199, #9776, #1972, #3877, #4730, #6668, #9875, #4249, #1226, #5886, #9953, #7341, #5931, #332, #8208, #7321, #2661, #1784, #4660, #4357, #1897, #2839, #1082, #8702 ) ) ;
#323 = EDGE_CURVE ( 'NONE', #8872, #4838, #1231, .T. ) ;
#324 = CARTESIAN_POINT ( 'NONE',  ( -5.812177826491105037, 10.00000000000000355, 3.933012701892163676 ) ) ;
#325 = CARTESIAN_POINT ( 'NONE',  ( -10.19839929293507375, 3.081249999044084920, 24.62111388749999108 ) ) ;
#326 = FACE_OUTER_BOUND ( 'NONE', #1511, .T. ) ;
#327 = CARTESIAN_POINT ( 'NONE',  ( 82.32050807568876394, 92.28203230275514102, 5.000000000000000000 ) ) ;
#328 = AXIS2_PLACEMENT_3D ( 'NONE', #8665, #3636, #7020 ) ;
#329 = CARTESIAN_POINT ( 'NONE',  ( -10.35533905932735621, 5.299999998088170905, 25.00000000000003197 ) ) ;
#330 = APPLICATION_CONTEXT ( 'automotive_design' ) ;
#331 = AXIS2_PLACEMENT_3D ( 'NONE', #9569, #2055, #5387 ) ;
#332 = ADVANCED_FACE ( 'NONE', ( #499 ), #4567, .T. ) ;
#333 = ORIENTED_EDGE ( 'NONE', *, *, #7900, .F. ) ;
#334 =( BOUNDED_CURVE ( )  B_SPLINE_CURVE ( 3, ( #9140, #1571, #4960, #8309 ),
 .UNSPECIFIED., .F., .F. ) 
 B_SPLINE_CURVE_WITH_KNOTS ( ( 4, 4 ),
 ( 2.284520705739657931, 2.356010155625178015 ),
 .UNSPECIFIED. ) 
 CURVE ( )  GEOMETRIC_REPRESENTATION_ITEM ( )  RATIONAL_B_SPLINE_CURVE ( ( 1.000000000000000000, 0.9995741502243209453, 0.9995741502243209453, 1.000000000000000000 ) ) 
 REPRESENTATION_ITEM ( '' )  );
#335 = EDGE_CURVE ( 'NONE', #6402, #2102, #10397, .T. ) ;
#336 = DIRECTION ( 'NONE',  ( 0.000000000000000000, 0.000000000000000000, -1.000000000000000000 ) ) ;
#337 = AXIS2_PLACEMENT_3D ( 'NONE', #6106, #5930, #7751 ) ;
#338 = CARTESIAN_POINT ( 'NONE',  ( -20.27611860449447079, 4.999999999999999112, 14.06603648214180247 ) ) ;
#339 = LINE ( 'NONE', #8784, #5857 ) ;
#340 = ORIENTED_EDGE ( 'NONE', *, *, #4019, .T. ) ;
#341 = CARTESIAN_POINT ( 'NONE',  ( 3.061616997868383043E-15, 5.000000000000000000, 25.00000000000000000 ) ) ;
#342 = DIRECTION ( 'NONE',  ( 1.000000000000000000, 0.000000000000000000, 0.000000000000000000 ) ) ;
#343 = CYLINDRICAL_SURFACE ( 'NONE', #9212, 12.77350269189627063 ) ;
#344 = CARTESIAN_POINT ( 'NONE',  ( -4.522825247065398226E-15, 3.968749999044084209, 24.62111388750000174 ) ) ;
#345 = CARTESIAN_POINT ( 'NONE',  ( 2.999999999999999112, -0.001000000000001000089, 19.75000000000000000 ) ) ;
#346 = VERTEX_POINT ( 'NONE', #9726 ) ;
#347 = PRODUCT_DEFINITION_FORMATION_WITH_SPECIFIED_SOURCE ( 'ANY', '', #361, .NOT_KNOWN. ) ;
#348 = DIRECTION ( 'NONE',  ( 0.000000000000000000, 0.000000000000000000, -1.000000000000000000 ) ) ;
#349 = CARTESIAN_POINT ( 'NONE',  ( -4.522825247065398226E-15, 1.968749999044084653, 24.62111388750000174 ) ) ;
#350 = CARTESIAN_POINT ( 'NONE',  ( -17.40975659021753330, 5.018749999044084475, 17.40975659021752975 ) ) ;
#351 = CARTESIAN_POINT ( 'NONE',  ( 17.67766952966368521, 4.875000000000000000, 17.67766952966369232 ) ) ;
#352 =( LENGTH_UNIT ( ) NAMED_UNIT ( * ) SI_UNIT ( .MILLI., .METRE. ) );
#353 = LINE ( 'NONE', #3726, #6158 ) ;
#354 = CARTESIAN_POINT ( 'NONE',  ( 6.145599950363597408, 19.66631150450990972, -3.355508642977475198 ) ) ;
#355 = DIRECTION ( 'NONE',  ( 0.000000000000000000, 1.000000000000000000, 0.000000000000000000 ) ) ;
#356 = PLANE ( 'NONE',  #3904 ) ;
#357 = VECTOR ( 'NONE', #4991, 1000.000000000000000 ) ;
#358 = CARTESIAN_POINT ( 'NONE',  ( 25.00000000000000000, 2.000000000000000000, 0.000000000000000000 ) ) ;
#359 = ORIENTED_EDGE ( 'NONE', *, *, #8815, .F. ) ;
#360 = ORIENTED_EDGE ( 'NONE', *, *, #10700, .T. ) ;
#361 = PRODUCT ( 'Removable Crank Handle & Arm Unit', 'Removable Crank Handle & Arm Unit', '', ( #7853 ) ) ;
#362 = LINE ( 'NONE', #3732, #5271 ) ;
#363 = AXIS2_PLACEMENT_3D ( 'NONE', #7383, #10762, #7726 ) ;
#364 = VECTOR ( 'NONE', #7348, 1000.000000000000000 ) ;
#365 = DIRECTION ( 'NONE',  ( -0.000000000000000000, -1.000000000000000000, -0.000000000000000000 ) ) ;
#366 = ORIENTED_EDGE ( 'NONE', *, *, #7588, .T. ) ;
#367 = DIRECTION ( 'NONE',  ( -1.000000000000000000, 5.551115123125781913E-15, 0.000000000000000000 ) ) ;
#368 = CARTESIAN_POINT ( 'NONE',  ( 15.60400172474260927, -0.001000000000001000089, -12.47307621135339062 ) ) ;
#369 = FACE_OUTER_BOUND ( 'NONE', #3316, .T. ) ;
#370 = CARTESIAN_POINT ( 'NONE',  ( -4.336808689942017736E-16, 20.00000000000000355, 6.999999999999997335 ) ) ;
#371 = DIRECTION ( 'NONE',  ( 0.000000000000000000, -0.000000000000000000, 1.000000000000000000 ) ) ;
#372 = CIRCLE ( 'NONE', #6199, 2.999999999999999112 ) ;
#373 = AXIS2_PLACEMENT_3D ( 'NONE', #6188, #3894, #6488 ) ;
#374 = ORIENTED_EDGE ( 'NONE', *, *, #8125, .T. ) ;
#375 = VERTEX_POINT ( 'NONE', #4612 ) ;
#376 = CARTESIAN_POINT ( 'NONE',  ( 17.40975659021752620, 4.268749999044084475, 17.40975659021753330 ) ) ;
#377 = EDGE_CURVE ( 'NONE', #6765, #3339, #3870, .T. ) ;
#378 = CARTESIAN_POINT ( 'NONE',  ( -7.171633369868398056, 7.781088913245559624, 11.42163336986824973 ) ) ;
#379 = CARTESIAN_POINT ( 'NONE',  ( 0.000000000000000000, 82.00000000000000000, 25.00000000000000000 ) ) ;
#380 = CYLINDRICAL_SURFACE ( 'NONE', #9214, 2.999999999999997335 ) ;
#381 = DIRECTION ( 'NONE',  ( 0.000000000000000000, 0.000000000000000000, 1.000000000000000000 ) ) ;
#382 = EDGE_CURVE ( 'NONE', #8258, #528, #7233, .T. ) ;
#383 = ORIENTED_EDGE ( 'NONE', *, *, #5717, .F. ) ;
#384 = AXIS2_PLACEMENT_3D ( 'NONE', #4121, #4890, #851 ) ;
#385 = DIRECTION ( 'NONE',  ( -0.000000000000000000, 1.000000000000000000, -0.000000000000000000 ) ) ;
#386 = CARTESIAN_POINT ( 'NONE',  ( -5.796693311223947376, 10.00000000000000355, 3.924072712834399734 ) ) ;
#387 = VERTEX_POINT ( 'NONE', #2812 ) ;
#388 = EDGE_CURVE ( 'NONE', #2139, #10138, #3054, .T. ) ;
#389 = AXIS2_PLACEMENT_3D ( 'NONE', #6634, #9992, #10835 ) ;
#390 = DIRECTION ( 'NONE',  ( 0.000000000000000000, 0.000000000000000000, 1.000000000000000000 ) ) ;
#391 = DIRECTION ( 'NONE',  ( 0.000000000000000000, 0.000000000000000000, 1.000000000000000000 ) ) ;
#392 = CARTESIAN_POINT ( 'NONE',  ( 15.60400172474269453, 25.00000000000000000, 12.47307621135327693 ) ) ;
#393 = ORIENTED_EDGE ( 'NONE', *, *, #10575, .T. ) ;
#394 = CARTESIAN_POINT ( 'NONE',  ( 24.62111388749999108, 2.156249999044084653, 10.19839929293507730 ) ) ;
#395 = LINE ( 'NONE', #6422, #1735 ) ;
#396 = EDGE_CURVE ( 'NONE', #5862, #7391, #2207, .T. ) ;
#397 = CIRCLE ( 'NONE', #8311, 6.999999999999997335 ) ;
#398 = EDGE_CURVE ( 'NONE', #963, #2292, #395, .T. ) ;
#399 = VERTEX_POINT ( 'NONE', #8842 ) ;
#400 = EDGE_LOOP ( 'NONE', ( #8892, #7575 ) ) ;
#401 = CIRCLE ( 'NONE', #10807, 6.999999999999997335 ) ;
#402 = CIRCLE ( 'NONE', #9394, 2.999999999999999112 ) ;
#403 = CARTESIAN_POINT ( 'NONE',  ( 0.000000000000000000, 20.00000000000000355, -6.999999999999997335 ) ) ;
#404 = CARTESIAN_POINT ( 'NONE',  ( -17.40975659021752975, 2.593749999044084653, -17.40975659021752975 ) ) ;
#405 = CIRCLE ( 'NONE', #9386, 2.000000000000000000 ) ;
#406 = CARTESIAN_POINT ( 'NONE',  ( 24.62111388750000174, 2.393749999044084475, 0.000000000000000000 ) ) ;
#407 = CARTESIAN_POINT ( 'NONE',  ( -25.00000000000000000, 3.437500000000000000, -10.35533905932738108 ) ) ;
#408 = FILL_AREA_STYLE ('',( #5487 ) ) ;
#409 = CIRCLE ( 'NONE', #8520, 0.1000000000000002554 ) ;
#410 = CARTESIAN_POINT ( 'NONE',  ( -17.67766952966368876, 0.9874999980881691286, -17.67766952966369232 ) ) ;
#411 = FACE_OUTER_BOUND ( 'NONE', #2991, .T. ) ;
#412 = AXIS2_PLACEMENT_3D ( 'NONE', #4846, #684, #4789 ) ;
#413 = DIRECTION ( 'NONE',  ( 1.000000000000000000, 0.000000000000000000, 0.000000000000000000 ) ) ;
#414 = EDGE_CURVE ( 'NONE', #5784, #652, #8731, .T. ) ;
#415 = CIRCLE ( 'NONE', #5701, 0.1000000000000002554 ) ;
#416 = VERTEX_POINT ( 'NONE', #5429 ) ;
#417 = VERTEX_POINT ( 'NONE', #2913 ) ;
#418 = ORIENTED_EDGE ( 'NONE', *, *, #7281, .F. ) ;
#419 = ORIENTED_EDGE ( 'NONE', *, *, #8806, .F. ) ;
#420 = CIRCLE ( 'NONE', #2878, 6.750000000000007994 ) ;
#421 = CARTESIAN_POINT ( 'NONE',  ( -25.00000000000001066, 0.5625000000000002220, 10.35533905932737397 ) ) ;
#422 = CARTESIAN_POINT ( 'NONE',  ( 1.499999999999999556, 83.00000000000000000, -1.500000000000000222 ) ) ;
#423 = CARTESIAN_POINT ( 'NONE',  ( -2.857142857142858983, 10.00000000000000355, -9.474358296526935064 ) ) ;
#424 = FACE_OUTER_BOUND ( 'NONE', #721, .T. ) ;
#425 = FACE_OUTER_BOUND ( 'NONE', #10415, .T. ) ;
#426 = PLANE ( 'NONE',  #3198 ) ;
#427 = CIRCLE ( 'NONE', #1301, 5.525000000000006573 ) ;
#428 = EDGE_LOOP ( 'NONE', ( #6689, #3315, #4054 ) ) ;
#429 = ORIENTED_EDGE ( 'NONE', *, *, #6271, .F. ) ;
#430 = ORIENTED_EDGE ( 'NONE', *, *, #4396, .T. ) ;
#431 = CARTESIAN_POINT ( 'NONE',  ( 1.400000000000001910, -1.415534356397074737E-16, -5.100000000000006750 ) ) ;
#432 = DIRECTION ( 'NONE',  ( -0.4999999999999919509, 0.000000000000000000, -0.8660254037844432595 ) ) ;
#433 = DIRECTION ( 'NONE',  ( 1.000000000000000000, 0.000000000000000000, 0.000000000000000000 ) ) ;
#434 = DIRECTION ( 'NONE',  ( 0.000000000000000000, -1.000000000000000000, 0.000000000000000000 ) ) ;
#435 = DIRECTION ( 'NONE',  ( 0.000000000000000000, 0.000000000000000000, 1.000000000000000000 ) ) ;
#436 = EDGE_CURVE ( 'NONE', #1816, #8189, #1374, .T. ) ;
#437 = ADVANCED_FACE ( 'NONE', ( #450 ), #10554, .F. ) ;
#438 = ORIENTED_EDGE ( 'NONE', *, *, #10019, .T. ) ;
#439 = EDGE_CURVE ( 'NONE', #3209, #9663, #8791, .T. ) ;
#440 = LINE ( 'NONE', #3807, #6013 ) ;
#441 = CARTESIAN_POINT ( 'NONE',  ( -4.592425496802574367E-15, 5.362499998088169129, 25.00000000000000000 ) ) ;
#442 = CARTESIAN_POINT ( 'NONE',  ( 1.507608415688466075E-15, 2.643749999044084920, -24.62111388750000174 ) ) ;
#443 = EDGE_LOOP ( 'NONE', ( #4090, #2708 ) ) ;
#444 = CARTESIAN_POINT ( 'NONE',  ( 24.62111388750000174, 5.218749999044084653, 0.000000000000000000 ) ) ;
#445 =( NAMED_UNIT ( * ) SI_UNIT ( $, .STERADIAN. ) SOLID_ANGLE_UNIT ( ) );
#446 = EDGE_CURVE ( 'NONE', #7282, #1433, #4666, .T. ) ;
#447 = CARTESIAN_POINT ( 'NONE',  ( 0.000000000000000000, 20.00000000000000355, 0.000000000000000000 ) ) ;
#448 = VERTEX_POINT ( 'NONE', #1591 ) ;
#449 = CARTESIAN_POINT ( 'NONE',  ( 24.62111388750000174, 4.281249999044084653, -10.19839929293505776 ) ) ;
#450 = FACE_OUTER_BOUND ( 'NONE', #4386, .T. ) ;
#451 = PRODUCT ( 'Upper Stainless Steel Body Shell', 'Upper Stainless Steel Body Shell', '', ( #5141 ) ) ;
#452 = ORIENTED_EDGE ( 'NONE', *, *, #7524, .T. ) ;
#453 = EDGE_CURVE ( 'NONE', #3864, #1133, #3229, .T. ) ;
#454 = CARTESIAN_POINT ( 'NONE',  ( 0.000000000000000000, 88.00000000000001421, 0.000000000000000000 ) ) ;
#455 = CARTESIAN_POINT ( 'NONE',  ( 1.507608415688466075E-15, 4.468749999044084653, -24.62111388750000174 ) ) ;
#456 = CARTESIAN_POINT ( 'NONE',  ( -17.40975659021752975, 1.768749999044084475, -17.40975659021752975 ) ) ;
#457 = VERTEX_POINT ( 'NONE', #3077 ) ;
#458 = CARTESIAN_POINT ( 'NONE',  ( -25.00000000000000000, 1.437500000000000000, -10.35533905932738108 ) ) ;
#459 = EDGE_CURVE ( 'NONE', #2069, #3931, #29, .T. ) ;
#460 = CARTESIAN_POINT ( 'NONE',  ( 0.000000000000000000, 88.00000000000001421, -4.999999999999997335 ) ) ;
#461 = DIRECTION ( 'NONE',  ( 0.000000000000000000, -0.000000000000000000, 1.000000000000000000 ) ) ;
#462 = PLANE ( 'NONE',  #6027 ) ;
#463 = CARTESIAN_POINT ( 'NONE',  ( 17.67766952966369232, 3.737499998088169573, -17.67766952966369232 ) ) ;
#464 = ORIENTED_EDGE ( 'NONE', *, *, #335, .T. ) ;
#465 = ORIENTED_EDGE ( 'NONE', *, *, #1592, .F. ) ;
#466 = CARTESIAN_POINT ( 'NONE',  ( -25.00000000000000000, 0.5000000000000000000, -3.061616997868383043E-15 ) ) ;
#467 = ADVANCED_FACE ( 'NONE', ( #4314 ), #3524, .F. ) ;
#468 = CARTESIAN_POINT ( 'NONE',  ( 2.500000000000000444, 1.000000000000002220, -0.5773502691896270633 ) ) ;
#469 = EDGE_CURVE ( 'NONE', #8735, #3294, #3407, .T. ) ;
#470 = CARTESIAN_POINT ( 'NONE',  ( -5.000000000000000000, 93.00000000000001421, 0.000000000000000000 ) ) ;
#471 = EDGE_LOOP ( 'NONE', ( #8532, #9181, #9575, #7189, #4997, #4095, #6051, #9424 ) ) ;
#472 = CARTESIAN_POINT ( 'NONE',  ( 0.000000000000000000, 20.00000000000000355, 0.000000000000000000 ) ) ;
#473 = CARTESIAN_POINT ( 'NONE',  ( -6.348076211353412823, 10.00000000000000355, 11.26313972081436532 ) ) ;
#474 = DIRECTION ( 'NONE',  ( 0.000000000000000000, 1.000000000000000000, 0.000000000000000000 ) ) ;
#475 = DIRECTION ( 'NONE',  ( 0.000000000000000000, 0.000000000000000000, 1.000000000000000000 ) ) ;
#476 = ORIENTED_EDGE ( 'NONE', *, *, #10844, .F. ) ;
#477 = ORIENTED_EDGE ( 'NONE', *, *, #2129, .T. ) ;
#478 = EDGE_CURVE ( 'NONE', #10364, #8941, #3461, .T. ) ;
#479 = MECHANICAL_DESIGN_GEOMETRIC_PRESENTATION_REPRESENTATION (  '', ( #10362 ), #8224 ) ;
#480 = CARTESIAN_POINT ( 'NONE',  ( -19.39162934935757931, 5.000000000000000888, 15.17115553405142947 ) ) ;
#481 = DIRECTION ( 'NONE',  ( 0.000000000000000000, 0.000000000000000000, -1.000000000000000000 ) ) ;
#482 = CARTESIAN_POINT ( 'NONE',  ( 2.500000000000000444, -1.000000000000003331, 0.5773502691896272854 ) ) ;
#483 = DIRECTION ( 'NONE',  ( 0.000000000000000000, 1.000000000000000000, 0.000000000000000000 ) ) ;
#484 = DIRECTION ( 'NONE',  ( -0.8660254037844451469, 0.000000000000000000, -0.4999999999999887312 ) ) ;
#485 = MECHANICAL_DESIGN_GEOMETRIC_PRESENTATION_REPRESENTATION (  '', ( #10900 ), #6489 ) ;
#486 = VECTOR ( 'NONE', #920, 1000.000000000000000 ) ;
#487 = ORIENTED_EDGE ( 'NONE', *, *, #845, .F. ) ;
#488 = ORIENTED_EDGE ( 'NONE', *, *, #2343, .T. ) ;
#489 = CARTESIAN_POINT ( 'NONE',  ( 19.75000000000001066, 28.00000000000000000, 2.999999999999927613 ) ) ;
#490 = CARTESIAN_POINT ( 'NONE',  ( 1.040834085586084257E-14, 90.00000000000001421, 5.000000000000000000 ) ) ;
#491 = CARTESIAN_POINT ( 'NONE',  ( -1.500000000000000444, 88.00000000000001421, 1.499999999999999778 ) ) ;
#492 = VERTEX_POINT ( 'NONE', #223 ) ;
#493 = DIRECTION ( 'NONE',  ( -0.000000000000000000, -1.000000000000000000, -0.000000000000000000 ) ) ;
#494 = PRESENTATION_STYLE_ASSIGNMENT (( #8112 ) ) ;
#495 = CARTESIAN_POINT ( 'NONE',  ( -12.69999999999998153, 0.000000000000000000, 0.000000000000000000 ) ) ;
#496 = ORIENTED_EDGE ( 'NONE', *, *, #2584, .T. ) ;
#497 = AXIS2_PLACEMENT_3D ( 'NONE', #5910, #6978, #9384 ) ;
#498 = CARTESIAN_POINT ( 'NONE',  ( 1.507608415688466075E-15, 1.468749999044084431, -24.62111388750000174 ) ) ;
#499 = FACE_OUTER_BOUND ( 'NONE', #9815, .T. ) ;
#500 = VERTEX_POINT ( 'NONE', #5316 ) ;
#501 = ORIENTED_EDGE ( 'NONE', *, *, #4410, .F. ) ;
#502 = VECTOR ( 'NONE', #9281, 999.9999999999998863 ) ;
#503 = CARTESIAN_POINT ( 'NONE',  ( 1.507608415688466075E-15, 2.468749999044085097, -24.62111388750000174 ) ) ;
#504 = CARTESIAN_POINT ( 'NONE',  ( 24.62111388749999463, 2.331249999044084031, 10.19839929293507730 ) ) ;
#505 = ORIENTED_EDGE ( 'NONE', *, *, #6617, .F. ) ;
#506 = CARTESIAN_POINT ( 'NONE',  ( 25.00000000000000000, 4.062500000000000000, -10.35533905932737753 ) ) ;
#507 = ADVANCED_FACE ( 'NONE', ( #3586 ), #10212, .F. ) ;
#508 = EDGE_CURVE ( 'NONE', #3100, #1857, #9259, .T. ) ;
#509 = DIRECTION ( 'NONE',  ( -0.000000000000000000, -1.000000000000000000, -0.000000000000000000 ) ) ;
#510 = CARTESIAN_POINT ( 'NONE',  ( 25.00000000000000000, 0.6749999980881690176, -10.35533905932737753 ) ) ;
#511 = DIRECTION ( 'NONE',  ( 0.000000000000000000, 0.000000000000000000, 1.000000000000000000 ) ) ;
#512 = LINE ( 'NONE', #7202, #5833 ) ;
#513 = ORIENTED_EDGE ( 'NONE', *, *, #1407, .T. ) ;
#514 = VERTEX_POINT ( 'NONE', #5086 ) ;
#515 = ORIENTED_EDGE ( 'NONE', *, *, #3176, .F. ) ;
#516 = ADVANCED_FACE ( 'NONE', ( #8437 ), #4251, .F. ) ;
#517 = CARTESIAN_POINT ( 'NONE',  ( 1.399999999999998579, 0.000000000000000000, 0.000000000000000000 ) ) ;
#518 = LINE ( 'NONE', #3202, #8425 ) ;
#519 = DIRECTION ( 'NONE',  ( 0.000000000000000000, 1.502202555303639631E-16, 1.000000000000000000 ) ) ;
#520 = EDGE_CURVE ( 'NONE', #5481, #3253, #2570, .T. ) ;
#521 = CARTESIAN_POINT ( 'NONE',  ( -5.000000000000000000, 93.00000000000001421, 5.000000000000000000 ) ) ;
#522 = DIRECTION ( 'NONE',  ( -0.000000000000000000, 1.000000000000000000, -0.000000000000000000 ) ) ;
#523 = CARTESIAN_POINT ( 'NONE',  ( 5.446152422706636465, 10.00000000000000355, -2.566987298107767490 ) ) ;
#524 = ORIENTED_EDGE ( 'NONE', *, *, #1672, .T. ) ;
#525 = EDGE_CURVE ( 'NONE', #5936, #10248, #7856, .T. ) ;
#526 = CIRCLE ( 'NONE', #1771, 12.77350269189627063 ) ;
#527 = CIRCLE ( 'NONE', #8986, 2.999999999999998668 ) ;
#528 = VERTEX_POINT ( 'NONE', #281 ) ;
#529 = DIRECTION ( 'NONE',  ( 0.000000000000000000, 0.000000000000000000, -1.000000000000000000 ) ) ;
#530 = DIRECTION ( 'NONE',  ( -0.000000000000000000, 1.000000000000000000, -0.000000000000000000 ) ) ;
#531 = LINE ( 'NONE', #8048, #2356 ) ;
#532 = VECTOR ( 'NONE', #6272, 1000.000000000000227 ) ;
#533 = EDGE_CURVE ( 'NONE', #8829, #4450, #8962, .T. ) ;
#534 = VECTOR ( 'NONE', #1707, 1000.000000000000000 ) ;
#535 = CARTESIAN_POINT ( 'NONE',  ( 1.040834085586084257E-14, 90.00000000000001421, 0.000000000000000000 ) ) ;
#536 = DIRECTION ( 'NONE',  ( 0.000000000000000000, 1.000000000000000000, 0.000000000000000000 ) ) ;
#537 = ORIENTED_EDGE ( 'NONE', *, *, #3535, .F. ) ;
#538 = EDGE_LOOP ( 'NONE', ( #10942, #1687, #7523, #476 ) ) ;
#539 = VECTOR ( 'NONE', #2027, 1000.000000000000000 ) ;
#540 = STYLED_ITEM ( 'NONE', ( #5737 ), #3340 ) ;
#541 = FILL_AREA_STYLE_COLOUR ( '', #3347 ) ;
#542 = CARTESIAN_POINT ( 'NONE',  ( 3.061616997868383043E-15, 85.00000000000000000, -25.00000000000000000 ) ) ;
#543 = CARTESIAN_POINT ( 'NONE',  ( 10.19839929293505953, 3.581249999044085364, -24.62111388750000174 ) ) ;
#544 = VERTEX_POINT ( 'NONE', #8636 ) ;
#545 = CARTESIAN_POINT ( 'NONE',  ( 19.75000000000000000, -0.001000000000001000089, -7.291468677852036884E-14 ) ) ;
#546 = CARTESIAN_POINT ( 'NONE',  ( -1.500000000000000444, 83.00000000000000000, 1.499999999999999778 ) ) ;
#547 = CARTESIAN_POINT ( 'NONE',  ( 24.62111388750000174, 1.281249999044084653, -10.19839929293505776 ) ) ;
#548 = DIRECTION ( 'NONE',  ( -0.000000000000000000, 1.000000000000000000, -0.000000000000000000 ) ) ;
#549 = ORIENTED_EDGE ( 'NONE', *, *, #6741, .T. ) ;
#550 = ORIENTED_EDGE ( 'NONE', *, *, #3080, .T. ) ;
#551 = VECTOR ( 'NONE', #10567, 1000.000000000000000 ) ;
#552 = CARTESIAN_POINT ( 'NONE',  ( -25.00000000000001421, 3.174999998088169129, 10.35533905932737397 ) ) ;
#553 = DIRECTION ( 'NONE',  ( 1.000000000000000000, 0.000000000000000000, 0.000000000000000000 ) ) ;
#554 = CARTESIAN_POINT ( 'NONE',  ( -24.62111388750000174, 3.893749999044084475, -3.015216831376932151E-15 ) ) ;
#555 = CARTESIAN_POINT ( 'NONE',  ( -4.592425496802574367E-15, 4.750000000000000000, 25.00000000000000000 ) ) ;
#556 = VECTOR ( 'NONE', #169, 1000.000000000000000 ) ;
#557 = CARTESIAN_POINT ( 'NONE',  ( -6.999999999999994671, 19.66631150450992749, -0.1668442477451158867 ) ) ;
#558 = CARTESIAN_POINT ( 'NONE',  ( -13.63990010960481492, 28.00000000000000000, 7.875000000000163425 ) ) ;
#559 = DIRECTION ( 'NONE',  ( 1.445602896647339163E-16, 0.000000000000000000, 1.000000000000000000 ) ) ;
#560 = DIRECTION ( 'NONE',  ( 0.000000000000000000, 0.000000000000000000, -1.000000000000000000 ) ) ;
#561 = VECTOR ( 'NONE', #1063, 1000.000000000000000 ) ;
#562 = ORIENTED_EDGE ( 'NONE', *, *, #9891, .F. ) ;
#563 = ORIENTED_EDGE ( 'NONE', *, *, #319, .T. ) ;
#564 = VERTEX_POINT ( 'NONE', #7642 ) ;
#565 = AXIS2_PLACEMENT_3D ( 'NONE', #8099, #5732, #433 ) ;
#566 = AXIS2_PLACEMENT_3D ( 'NONE', #6788, #151, #987 ) ;
#567 = EDGE_CURVE ( 'NONE', #9293, #10413, #10782, .T. ) ;
#568 = CARTESIAN_POINT ( 'NONE',  ( 25.00000000000000000, 4.000000000000000000, 0.000000000000000000 ) ) ;
#569 = AXIS2_PLACEMENT_3D ( 'NONE', #4292, #5896, #6784 ) ;
#570 = DIRECTION ( 'NONE',  ( -1.000000000000000000, 0.000000000000000000, 0.000000000000000000 ) ) ;
#571 =( NAMED_UNIT ( * ) PLANE_ANGLE_UNIT ( ) SI_UNIT ( $, .RADIAN. ) );
#572 = AXIS2_PLACEMENT_3D ( 'NONE', #5272, #10857, #4120 ) ;
#573 = CARTESIAN_POINT ( 'NONE',  ( 3.058047309050023088, 10.00000000000000355, -6.296693311223907408 ) ) ;
#574 = EDGE_CURVE ( 'NONE', #8829, #3039, #9473, .T. ) ;
#575 = DIRECTION ( 'NONE',  ( 0.000000000000000000, 0.000000000000000000, -1.000000000000000000 ) ) ;
#576 = AXIS2_PLACEMENT_3D ( 'NONE', #6748, #5973, #10110 ) ;
#577 = CARTESIAN_POINT ( 'NONE',  ( -15.60400172474251690, 28.00000000000000000, 12.47307621135349720 ) ) ;
#578 = CARTESIAN_POINT ( 'NONE',  ( 1.500000000000001332, -2.053912595556539452E-16, -7.400000000000007461 ) ) ;
#579 = ORIENTED_EDGE ( 'NONE', *, *, #4051, .T. ) ;
#580 = ORIENTED_EDGE ( 'NONE', *, *, #5350, .F. ) ;
#581 = AXIS2_PLACEMENT_3D ( 'NONE', #6035, #5977, #10168 ) ;
#582 = EDGE_LOOP ( 'NONE', ( #4342, #8954, #2146, #5276, #930 ) ) ;
#583 = CIRCLE ( 'NONE', #4834, 6.999999999999997335 ) ;
#584 = ORIENTED_EDGE ( 'NONE', *, *, #5586, .F. ) ;
#585 = EDGE_CURVE ( 'NONE', #6763, #4029, #1905, .T. ) ;
#586 = ORIENTED_EDGE ( 'NONE', *, *, #567, .T. ) ;
#587 = AXIS2_PLACEMENT_3D ( 'NONE', #4145, #5850, #2623 ) ;
#588 = DIRECTION ( 'NONE',  ( -1.000000000000000000, 0.000000000000000000, -1.047444401652940007E-14 ) ) ;
#589 = CIRCLE ( 'NONE', #3780, 22.00000000000000355 ) ;
#590 = DIRECTION ( 'NONE',  ( -1.000000000000000000, 0.000000000000000000, 0.000000000000000000 ) ) ;
#591 = EDGE_CURVE ( 'NONE', #811, #698, #1969, .T. ) ;
#592 = PLANE ( 'NONE',  #2028 ) ;
#593 = DIRECTION ( 'NONE',  ( -0.000000000000000000, -1.000000000000000000, -0.000000000000000000 ) ) ;
#594 = DIRECTION ( 'NONE',  ( 0.000000000000000000, 1.000000000000000000, 0.000000000000000000 ) ) ;
#595 = AXIS2_PLACEMENT_3D ( 'NONE', #2399, #9367, #7543 ) ;
#596 = ORIENTED_EDGE ( 'NONE', *, *, #10438, .T. ) ;
#597 = ORIENTED_EDGE ( 'NONE', *, *, #2649, .F. ) ;
#598 = LINE ( 'NONE', #3011, #2601 ) ;
#599 =( NAMED_UNIT ( * ) PLANE_ANGLE_UNIT ( ) SI_UNIT ( $, .RADIAN. ) );
#600 = CARTESIAN_POINT ( 'NONE',  ( -3.924072712834378862, 19.03096903053431888, -5.796693311223959810 ) ) ;
#601 = CARTESIAN_POINT ( 'NONE',  ( -24.62111388750000884, 2.956249999044084475, 10.19839929293505421 ) ) ;
#602 = ADVANCED_FACE ( 'NONE', ( #6052 ), #6853, .T. ) ;
#603 = ORIENTED_EDGE ( 'NONE', *, *, #8062, .F. ) ;
#604 = LINE ( 'NONE', #4915, #6711 ) ;
#605 = DIRECTION ( 'NONE',  ( 0.000000000000000000, 0.000000000000000000, 1.000000000000000000 ) ) ;
#606 = LINE ( 'NONE', #10829, #1633 ) ;
#607 = EDGE_LOOP ( 'NONE', ( #9268, #5348, #7147, #5082, #6374 ) ) ;
#608 = ORIENTED_EDGE ( 'NONE', *, *, #5350, .T. ) ;
#609 = CARTESIAN_POINT ( 'NONE',  ( -25.00000000000000000, 5.112499998088170017, -3.061616997868383043E-15 ) ) ;
#610 = CARTESIAN_POINT ( 'NONE',  ( -20.63749999999999929, 0.000000000000000000, 0.000000000000000000 ) ) ;
#611 = CARTESIAN_POINT ( 'NONE',  ( 24.62111388750000174, 5.393749999044085364, 0.000000000000000000 ) ) ;
#612 = EDGE_LOOP ( 'NONE', ( #729, #7297, #168, #8289 ) ) ;
#613 = LINE ( 'NONE', #784, #5147 ) ;
#614 =( BOUNDED_CURVE ( )  B_SPLINE_CURVE ( 2, ( #3089, #1344, #5599, #8078, #6437, #9838, #463, #1440, #10520 ),
 .UNSPECIFIED., .F., .F. ) 
 B_SPLINE_CURVE_WITH_KNOTS ( ( 3, 2, 2, 2, 3 ),
 ( 0.5500000000000000444, 0.5749999999999999556, 0.5999999999999999778, 0.6250000000000000000, 0.6500000000000000222 ),
 .UNSPECIFIED. ) 
 CURVE ( )  GEOMETRIC_REPRESENTATION_ITEM ( )  RATIONAL_B_SPLINE_CURVE ( ( 1.000000000000000000, 0.9238795325112867385, 1.000000000000000000, 0.9238795325112867385, 1.000000000000000000, 0.9238795325112867385, 1.000000000000000000, 0.9238795325112867385, 1.000000000000000000 ) ) 
 REPRESENTATION_ITEM ( '' )  );
#615 = PLANE ( 'NONE',  #10718 ) ;
#616 = CARTESIAN_POINT ( 'NONE',  ( 25.00000000000000000, 1.674999998088169351, -10.35533905932737753 ) ) ;
#617 = DIRECTION ( 'NONE',  ( -0.5000000000000009992, -0.8660254037844380415, -5.237222008264710288E-15 ) ) ;
#618 = CARTESIAN_POINT ( 'NONE',  ( 8.660254037844401509, 90.00000000000001421, -5.000000000000000000 ) ) ;
#619 = ORIENTED_EDGE ( 'NONE', *, *, #10120, .T. ) ;
#620 = VERTEX_POINT ( 'NONE', #910 ) ;
#621 = ORIENTED_EDGE ( 'NONE', *, *, #1452, .F. ) ;
#622 = ORIENTED_EDGE ( 'NONE', *, *, #2384, .T. ) ;
#623 = UNCERTAINTY_MEASURE_WITH_UNIT (LENGTH_MEASURE( 1.000000000000000082E-05 ), #723, 'distance_accuracy_value', 'NONE');
#624 = CARTESIAN_POINT ( 'NONE',  ( -10.19839929293505776, 0.5312499990440845421, -24.62111388750000174 ) ) ;
#625 = ORIENTED_EDGE ( 'NONE', *, *, #3191, .F. ) ;
#626 = CARTESIAN_POINT ( 'NONE',  ( 6.296693311223917178, 10.00000000000000355, -3.058047309050000440 ) ) ;
#627 = CYLINDRICAL_SURFACE ( 'NONE', #9189, 25.00000000000000000 ) ;
#628 = ADVANCED_FACE ( 'NONE', ( #4398 ), #5994, .T. ) ;
#629 = CARTESIAN_POINT ( 'NONE',  ( 24.62111388749999463, 2.156249999044085097, 10.19839929293507730 ) ) ;
#630 = CARTESIAN_POINT ( 'NONE',  ( 1.530808498934191521E-15, 3.250000000000000444, -25.00000000000000000 ) ) ;
#631 = VERTEX_POINT ( 'NONE', #10241 ) ;
#632 = EDGE_LOOP ( 'NONE', ( #359, #6659, #4247, #3379 ) ) ;
#633 = ORIENTED_EDGE ( 'NONE', *, *, #8885, .F. ) ;
#634 = VERTEX_POINT ( 'NONE', #10183 ) ;
#635 = ORIENTED_EDGE ( 'NONE', *, *, #6976, .T. ) ;
#636 = EDGE_CURVE ( 'NONE', #9541, #9951, #1793, .T. ) ;
#637 = EDGE_LOOP ( 'NONE', ( #10358, #10252, #5332, #5163 ) ) ;
#638 = DIRECTION ( 'NONE',  ( 0.000000000000000000, -2.775557561562891351E-17, -1.000000000000000000 ) ) ;
#639 = CARTESIAN_POINT ( 'NONE',  ( -3.644491357022560329, 19.66631150450991328, 5.978755702618518519 ) ) ;
#640 = CARTESIAN_POINT ( 'NONE',  ( -2.999999999999996447, 25.00000000000000000, 19.75000000000000000 ) ) ;
#641 = EDGE_CURVE ( 'NONE', #2931, #7240, #5287, .T. ) ;
#642 = CARTESIAN_POINT ( 'NONE',  ( 17.67766952966368521, 3.875000000000000000, 17.67766952966369232 ) ) ;
#643 = ADVANCED_FACE ( 'NONE', ( #9413 ), #7049, .T. ) ;
#644 = CARTESIAN_POINT ( 'NONE',  ( -12.13990010960501031, -0.001000000000001000089, -10.47307621135320410 ) ) ;
#645 = EDGE_LOOP ( 'NONE', ( #3984, #3500, #6506, #4878 ) ) ;
#646 = EDGE_CURVE ( 'NONE', #6058, #5812, #132, .T. ) ;
#647 = ORIENTED_EDGE ( 'NONE', *, *, #6126, .F. ) ;
#648 = FACE_OUTER_BOUND ( 'NONE', #8082, .T. ) ;
#649 = LINE ( 'NONE', #7380, #8128 ) ;
#650 = SURFACE_STYLE_USAGE ( .BOTH. , #5631 ) ;
#651 = CARTESIAN_POINT ( 'NONE',  ( 24.62111388750000174, 3.456249999044084920, -10.19839929293505776 ) ) ;
#652 = VERTEX_POINT ( 'NONE', #1852 ) ;
#653 = DIRECTION ( 'NONE',  ( 0.000000000000000000, -0.000000000000000000, 1.000000000000000000 ) ) ;
#654 = CARTESIAN_POINT ( 'NONE',  ( 0.000000000000000000, 0.000000000000000000, 0.000000000000000000 ) ) ;
#655 = DIRECTION ( 'NONE',  ( -0.000000000000000000, -1.000000000000000000, -0.000000000000000000 ) ) ;
#656 = ORIENTED_EDGE ( 'NONE', *, *, #8957, .F. ) ;
#657 = CARTESIAN_POINT ( 'NONE',  ( -17.67766952966369232, 1.625000000000000222, 17.67766952966368876 ) ) ;
#658 = EDGE_CURVE ( 'NONE', #10864, #2380, #8577, .T. ) ;
#659 = CARTESIAN_POINT ( 'NONE',  ( -17.40975659021753330, 1.843749999044084653, 17.40975659021752975 ) ) ;
#660 = EDGE_LOOP ( 'NONE', ( #8805, #3492, #5444 ) ) ;
#661 = ADVANCED_FACE ( 'NONE', ( #7154 ), #8753, .F. ) ;
#662 = CARTESIAN_POINT ( 'NONE',  ( -24.62111388750000884, 0.9562499990440846975, 10.19839929293505421 ) ) ;
#663 = CARTESIAN_POINT ( 'NONE',  ( 67.32050807568876394, 89.28203230275514102, 5.000000000000000000 ) ) ;
#664 = VECTOR ( 'NONE', #5477, 1000.000000000000000 ) ;
#665 = CARTESIAN_POINT ( 'NONE',  ( 10.19839929293506486, 1.031249999044084653, 24.62111388749999819 ) ) ;
#666 = CARTESIAN_POINT ( 'NONE',  ( -20.63749999999999929, 8.637664692995951295E-16, 5.750000000000006217 ) ) ;
#667 =( NAMED_UNIT ( * ) SI_UNIT ( $, .STERADIAN. ) SOLID_ANGLE_UNIT ( ) );
#668 = CARTESIAN_POINT ( 'NONE',  ( -7.875000000000116351, -0.001000000000001000089, -13.63990010960484334 ) ) ;
#669 = LINE ( 'NONE', #7401, #7772 ) ;
#670 = DIRECTION ( 'NONE',  ( 0.000000000000000000, -2.775557561562888270E-17, -1.000000000000000000 ) ) ;
#671 = DIRECTION ( 'NONE',  ( -0.5000000000000009992, -0.8660254037844380415, -5.237222008264710288E-15 ) ) ;
#672 = CIRCLE ( 'NONE', #9503, 2.000000000000000000 ) ;
#673 = APPLICATION_CONTEXT ( 'automotive_design' ) ;
#674 = ADVANCED_FACE ( 'NONE', ( #2881 ), #5596, .F. ) ;
#675 = CIRCLE ( 'NONE', #6169, 15.00000000000000178 ) ;
#676 = ORIENTED_EDGE ( 'NONE', *, *, #388, .T. ) ;
#677 = ORIENTED_EDGE ( 'NONE', *, *, #2132, .T. ) ;
#678 = ORIENTED_EDGE ( 'NONE', *, *, #6885, .F. ) ;
#679 = ORIENTED_EDGE ( 'NONE', *, *, #641, .F. ) ;
#680 =( BOUNDED_CURVE ( )  B_SPLINE_CURVE ( 3, ( #1827, #826, #9316, #8327 ),
 .UNSPECIFIED., .F., .F. ) 
 B_SPLINE_CURVE_WITH_KNOTS ( ( 4, 4 ),
 ( 2.284520705739662816, 2.356010155625183344 ),
 .UNSPECIFIED. ) 
 CURVE ( )  GEOMETRIC_REPRESENTATION_ITEM ( )  RATIONAL_B_SPLINE_CURVE ( ( 1.000000000000000000, 0.9995741502243209453, 0.9995741502243209453, 1.000000000000000000 ) ) 
 REPRESENTATION_ITEM ( '' )  );
#681 = CARTESIAN_POINT ( 'NONE',  ( -4.522825247065398226E-15, 0.9687499990440845421, 24.62111388750000174 ) ) ;
#682 = DIRECTION ( 'NONE',  ( 0.8660254037844399289, 0.000000000000000000, 0.4999999999999978351 ) ) ;
#683 = CARTESIAN_POINT ( 'NONE',  ( -18.60400172474257730, 25.00000000000000000, 7.276923788646904256 ) ) ;
#684 = DIRECTION ( 'NONE',  ( 0.000000000000000000, 1.000000000000000000, 0.000000000000000000 ) ) ;
#685 = FACE_OUTER_BOUND ( 'NONE', #2794, .T. ) ;
#686 = CARTESIAN_POINT ( 'NONE',  ( 24.62111388750000174, 3.218749999044084653, 0.000000000000000000 ) ) ;
#687 = CARTESIAN_POINT ( 'NONE',  ( -1.400000000000001910, -1.415534356397074737E-16, -5.100000000000006750 ) ) ;
#688 = EDGE_CURVE ( 'NONE', #7766, #10229, #10434, .T. ) ;
#689 = VERTEX_POINT ( 'NONE', #7976 ) ;
#690 = ORIENTED_EDGE ( 'NONE', *, *, #10232, .T. ) ;
#691 = PLANE ( 'NONE',  #569 ) ;
#692 = CARTESIAN_POINT ( 'NONE',  ( 5.796693311223918066, 10.00000000000000355, -3.924072712834439702 ) ) ;
#693 = CARTESIAN_POINT ( 'NONE',  ( -1.500000000000000444, 83.00000000000000000, -1.500000000000000222 ) ) ;
#694 = DIRECTION ( 'NONE',  ( 0.5000000000000009992, 0.8660254037844380415, 5.237222008264710288E-15 ) ) ;
#695 = DIRECTION ( 'NONE',  ( 0.000000000000000000, 0.000000000000000000, -1.000000000000000000 ) ) ;
#696 = AXIS2_PLACEMENT_3D ( 'NONE', #5366, #10629, #1398 ) ;
#697 = VECTOR ( 'NONE', #9069, 1000.000000000000000 ) ;
#698 = VERTEX_POINT ( 'NONE', #1341 ) ;
#699 = EDGE_CURVE ( 'NONE', #8354, #9358, #9835, .T. ) ;
#700 = AXIS2_PLACEMENT_3D ( 'NONE', #7174, #7076, #7125 ) ;
#701 = LINE ( 'NONE', #1368, #8 ) ;
#702 = SURFACE_STYLE_FILL_AREA ( #3978 ) ;
#703 = AXIS2_PLACEMENT_3D ( 'NONE', #3703, #2954, #6358 ) ;
#704 = CARTESIAN_POINT ( 'NONE',  ( -17.40975659021752975, 0.7687499990440845865, -17.40975659021752975 ) ) ;
#705 = EDGE_LOOP ( 'NONE', ( #4344, #10523, #4176, #8992 ) ) ;
#706 = LINE ( 'NONE', #4869, #4614 ) ;
#707 = PRODUCT_CONTEXT ( 'NONE', #3857, 'mechanical' ) ;
#708 = PLANE ( 'NONE',  #6776 ) ;
#709 = CARTESIAN_POINT ( 'NONE',  ( 67.07963283087528339, 92.45240317130979690, -5.000000000000000000 ) ) ;
#710 = CARTESIAN_POINT ( 'NONE',  ( -4.522825247065398226E-15, 0.9687499990440845421, 24.62111388750000174 ) ) ;
#711 = EDGE_CURVE ( 'NONE', #8862, #6537, #6673, .T. ) ;
#712 = ORIENTED_EDGE ( 'NONE', *, *, #4302, .T. ) ;
#713 = VECTOR ( 'NONE', #2272, 1000.000000000000000 ) ;
#714 = ORIENTED_EDGE ( 'NONE', *, *, #5386, .T. ) ;
#715 = ADVANCED_BREP_SHAPE_REPRESENTATION ( '', ( #10733, #7040 ), #6327 ) ;
#716 = VERTEX_POINT ( 'NONE', #6382 ) ;
#717 = ADVANCED_FACE ( 'NONE', ( #1386 ), #8129, .T. ) ;
#718 = CARTESIAN_POINT ( 'NONE',  ( -10.35533905932737575, 3.924999998088169129, -25.00000000000000000 ) ) ;
#719 = DIRECTION ( 'NONE',  ( -0.000000000000000000, -1.000000000000000000, -0.000000000000000000 ) ) ;
#720 = CARTESIAN_POINT ( 'NONE',  ( -10.19839929293505776, 3.531249999044084653, -24.62111388750000174 ) ) ;
#721 = EDGE_LOOP ( 'NONE', ( #2374, #8932, #8644, #8469 ) ) ;
#722 = CARTESIAN_POINT ( 'NONE',  ( 15.13990010960488952, 28.00000000000000000, -5.276923788646758595 ) ) ;
#723 =( LENGTH_UNIT ( ) NAMED_UNIT ( * ) SI_UNIT ( .MILLI., .METRE. ) );
#724 = LINE ( 'NONE', #5809, #357 ) ;
#725 = FACE_OUTER_BOUND ( 'NONE', #3287, .T. ) ;
#726 = CARTESIAN_POINT ( 'NONE',  ( 0.000000000000000000, 10.00000000000000355, 0.000000000000000000 ) ) ;
#727 = EDGE_CURVE ( 'NONE', #698, #5070, #8800, .T. ) ;
#728 = VECTOR ( 'NONE', #9849, 1000.000000000000000 ) ;
#729 = ORIENTED_EDGE ( 'NONE', *, *, #3055, .T. ) ;
#730 = ORIENTED_EDGE ( 'NONE', *, *, #9628, .F. ) ;
#731 = ORIENTED_EDGE ( 'NONE', *, *, #3404, .F. ) ;
#732 = ORIENTED_EDGE ( 'NONE', *, *, #949, .T. ) ;
#733 = PRODUCT_DEFINITION_CONTEXT ( 'detailed design', #2156, 'design' ) ;
#734 = VECTOR ( 'NONE', #3164, 999.9999999999998863 ) ;
#735 = CARTESIAN_POINT ( 'NONE',  ( 24.62111388749999463, 3.331249999044084920, 10.19839929293507730 ) ) ;
#736 = DIRECTION ( 'NONE',  ( 0.000000000000000000, 0.000000000000000000, 1.000000000000000000 ) ) ;
#737 = LINE ( 'NONE', #6601, #10727 ) ;
#738 = EDGE_CURVE ( 'NONE', #69, #8014, #353, .T. ) ;
#739 = AXIS2_PLACEMENT_3D ( 'NONE', #4438, #9619, #4506 ) ;
#740 = CARTESIAN_POINT ( 'NONE',  ( -2.850480947161592393, 19.75000000000000000, -5.937177826491103261 ) ) ;
#741 = FACE_BOUND ( 'NONE', #6305, .T. ) ;
#742 = FACE_OUTER_BOUND ( 'NONE', #10182, .T. ) ;
#743 = CARTESIAN_POINT ( 'NONE',  ( -24.62111388750000884, 0.7812499990440845421, 10.19839929293505421 ) ) ;
#744 = CARTESIAN_POINT ( 'NONE',  ( 0.000000000000000000, 5.919319018694160373E-16, -6.250000000000007105 ) ) ;
#745 = ORIENTED_EDGE ( 'NONE', *, *, #6957, .T. ) ;
#746 = CIRCLE ( 'NONE', #6240, 2.999999999999999112 ) ;
#747 = ORIENTED_EDGE ( 'NONE', *, *, #1322, .F. ) ;
#748 = VERTEX_POINT ( 'NONE', #2062 ) ;
#749 = AXIS2_PLACEMENT_3D ( 'NONE', #4855, #8981, #8097 ) ;
#750 = EDGE_LOOP ( 'NONE', ( #8386, #3432 ) ) ;
#751 = VECTOR ( 'NONE', #9383, 1000.000000000000000 ) ;
#752 = VECTOR ( 'NONE', #4466, 1000.000000000000000 ) ;
#753 = CARTESIAN_POINT ( 'NONE',  ( 0.000000000000000000, 20.00000000000000355, 0.000000000000000000 ) ) ;
#754 = DIRECTION ( 'NONE',  ( 0.000000000000000000, 1.000000000000000000, 0.000000000000000000 ) ) ;
#755 = FACE_OUTER_BOUND ( 'NONE', #919, .T. ) ;
#756 = CARTESIAN_POINT ( 'NONE',  ( 1.400000000000001910, 0.000000000000000000, 0.000000000000000000 ) ) ;
#757 = CARTESIAN_POINT ( 'NONE',  ( 3.924072712834419718, 10.00000000000000355, 5.796693311223933165 ) ) ;
#758 = AXIS2_PLACEMENT_3D ( 'NONE', #2810, #6208, #9567 ) ;
#759 = AXIS2_PLACEMENT_3D ( 'NONE', #1982, #9602, #6241 ) ;
#760 = ORIENTED_EDGE ( 'NONE', *, *, #1166, .T. ) ;
#761 = VECTOR ( 'NONE', #8157, 1000.000000000000000 ) ;
#762 = VECTOR ( 'NONE', #6178, 1000.000000000000114 ) ;
#763 = DIRECTION ( 'NONE',  ( 0.000000000000000000, -1.000000000000000000, 0.000000000000000000 ) ) ;
#764 = CARTESIAN_POINT ( 'NONE',  ( 1.530808498934191521E-15, 4.862499998088169129, -25.00000000000000000 ) ) ;
#765 = LINE ( 'NONE', #10659, #3839 ) ;
#766 = CARTESIAN_POINT ( 'NONE',  ( 0.000000000000000000, 82.00000000000000000, 0.000000000000000000 ) ) ;
#767 = ORIENTED_EDGE ( 'NONE', *, *, #8949, .F. ) ;
#768 = LINE ( 'NONE', #8263, #2119 ) ;
#769 =( LENGTH_UNIT ( ) NAMED_UNIT ( * ) SI_UNIT ( .MILLI., .METRE. ) );
#770 = DIRECTION ( 'NONE',  ( 0.000000000000000000, 0.000000000000000000, -1.000000000000000000 ) ) ;
#771 = VECTOR ( 'NONE', #10871, 1000.000000000000000 ) ;
#772 = FACE_OUTER_BOUND ( 'NONE', #7291, .T. ) ;
#773 = CARTESIAN_POINT ( 'NONE',  ( 0.000000000000000000, 7.000000000000003553, -4.500000000000000888 ) ) ;
#774 = ADVANCED_FACE ( 'NONE', ( #4722 ), #8028, .F. ) ;
#775 = CIRCLE ( 'NONE', #8006, 6.999999999999997335 ) ;
#776 = EDGE_LOOP ( 'NONE', ( #10832, #8415, #8860, #10571 ) ) ;
#777 = EDGE_LOOP ( 'NONE', ( #3949, #5123, #7353, #340, #8376, #4998 ) ) ;
#778 = EDGE_CURVE ( 'NONE', #2292, #917, #6434, .T. ) ;
#779 = CARTESIAN_POINT ( 'NONE',  ( -17.40975659021752975, 0.7687499990440845865, -17.40975659021752975 ) ) ;
#780 = DIRECTION ( 'NONE',  ( -0.000000000000000000, 1.000000000000000000, -0.000000000000000000 ) ) ;
#781 = CARTESIAN_POINT ( 'NONE',  ( 24.62111388750000174, 1.218749999044084431, 0.000000000000000000 ) ) ;
#782 = LINE ( 'NONE', #4259, #4639 ) ;
#783 = ORIENTED_EDGE ( 'NONE', *, *, #7325, .T. ) ;
#784 = CARTESIAN_POINT ( 'NONE',  ( -5.437177826491026877, 19.75000000000000355, -3.716506350946172876 ) ) ;
#785 = SURFACE_STYLE_FILL_AREA ( #5806 ) ;
#786 = CARTESIAN_POINT ( 'NONE',  ( 0.000000000000000000, 82.00000000000000000, 0.000000000000000000 ) ) ;
#787 = CARTESIAN_POINT ( 'NONE',  ( 0.000000000000000000, 26.20172123805511788, 0.000000000000000000 ) ) ;
#788 = LINE ( 'NONE', #4206, #9032 ) ;
#789 = DIRECTION ( 'NONE',  ( 1.000000000000000000, 0.000000000000000000, 0.000000000000000000 ) ) ;
#790 = CARTESIAN_POINT ( 'NONE',  ( -12.47307621135311351, 28.00000000000000000, 15.60400172474282599 ) ) ;
#791 = EDGE_CURVE ( 'NONE', #2046, #346, #7043, .T. ) ;
#792 = EDGE_CURVE ( 'NONE', #3303, #9988, #3484, .T. ) ;
#793 = ORIENTED_EDGE ( 'NONE', *, *, #8651, .F. ) ;
#794 = EDGE_LOOP ( 'NONE', ( #9614, #452, #10633, #7368 ) ) ;
#795 = VERTEX_POINT ( 'NONE', #460 ) ;
#796 = ORIENTED_EDGE ( 'NONE', *, *, #6662, .F. ) ;
#797 = EDGE_CURVE ( 'NONE', #6584, #9935, #4622, .T. ) ;
#798 = CARTESIAN_POINT ( 'NONE',  ( 24.62111388750000174, 3.393749999044084475, 0.000000000000000000 ) ) ;
#799 = CARTESIAN_POINT ( 'NONE',  ( 17.40975659021752975, 1.343749999044084653, -17.40975659021752975 ) ) ;
#800 = CARTESIAN_POINT ( 'NONE',  ( 0.000000000000000000, -0.5289809421253948152, -22.00000000000000355 ) ) ;
#801 = LINE ( 'NONE', #740, #2804 ) ;
#802 = FACE_BOUND ( 'NONE', #1466, .T. ) ;
#803 = DIRECTION ( 'NONE',  ( -0.4999999999999886757, 0.000000000000000000, 0.8660254037844452579 ) ) ;
#804 = CARTESIAN_POINT ( 'NONE',  ( 1.507608415688466075E-15, 2.468749999044085097, -24.62111388750000174 ) ) ;
#805 = PLANE ( 'NONE',  #10636 ) ;
#806 = VERTEX_POINT ( 'NONE', #6323 ) ;
#807 = ORIENTED_EDGE ( 'NONE', *, *, #2469, .F. ) ;
#808 = ORIENTED_EDGE ( 'NONE', *, *, #2666, .F. ) ;
#809 = ORIENTED_EDGE ( 'NONE', *, *, #4102, .F. ) ;
#810 = EDGE_CURVE ( 'NONE', #5184, #1232, #9685, .T. ) ;
#811 = VERTEX_POINT ( 'NONE', #2974 ) ;
#812 = EDGE_CURVE ( 'NONE', #8587, #10544, #2924, .T. ) ;
#813 = CARTESIAN_POINT ( 'NONE',  ( -0.5590169943749458970, 8.637664692995941434E-16, 5.750000000000000000 ) ) ;
#814 = DIRECTION ( 'NONE',  ( 0.8660254037844344888, 0.000000000000000000, -0.5000000000000074385 ) ) ;
#815 = CARTESIAN_POINT ( 'NONE',  ( 0.000000000000000000, 85.00000000000000000, -25.00000000000000000 ) ) ;
#816 = DIRECTION ( 'NONE',  ( 0.8838834764831839941, 0.3535533905932757293, 0.3061862178478963470 ) ) ;
#817 = DIRECTION ( 'NONE',  ( 0.7559289460184611675, 0.000000000000000000, -0.6546536707079694262 ) ) ;
#818 = ADVANCED_FACE ( 'NONE', ( #6639 ), #615, .F. ) ;
#819 = ORIENTED_EDGE ( 'NONE', *, *, #6227, .T. ) ;
#820 = FACE_BOUND ( 'NONE', #8065, .T. ) ;
#821 = FACE_OUTER_BOUND ( 'NONE', #5736, .T. ) ;
#822 = CYLINDRICAL_SURFACE ( 'NONE', #4192, 5.999999999999999112 ) ;
#823 = FACE_OUTER_BOUND ( 'NONE', #9392, .T. ) ;
#824 = VERTEX_POINT ( 'NONE', #3298 ) ;
#825 = CYLINDRICAL_SURFACE ( 'NONE', #10417, 25.00000000000000000 ) ;
#826 = CARTESIAN_POINT ( 'NONE',  ( -3.644491357022439537, 19.66631150450991328, -5.978755702618592238 ) ) ;
#827 = DIRECTION ( 'NONE',  ( -0.3061862178479081154, 0.3535533905932724541, 0.8838834764831812185 ) ) ;
#828 = DIRECTION ( 'NONE',  ( 0.000000000000000000, -0.000000000000000000, 1.000000000000000000 ) ) ;
#829 = ORIENTED_EDGE ( 'NONE', *, *, #10797, .T. ) ;
#830 = CARTESIAN_POINT ( 'NONE',  ( 1.507608415688466075E-15, 3.643749999044084920, -24.62111388750000174 ) ) ;
#831 = DIRECTION ( 'NONE',  ( -3.469446951953617344E-15, 0.000000000000000000, 1.000000000000000000 ) ) ;
#832 = CARTESIAN_POINT ( 'NONE',  ( -17.40975659021753330, 0.8437499990440846531, 17.40975659021752975 ) ) ;
#833 = FACE_OUTER_BOUND ( 'NONE', #9928, .T. ) ;
#834 = EDGE_LOOP ( 'NONE', ( #2403, #1954, #8733, #10680 ) ) ;
#835 = DIRECTION ( 'NONE',  ( 0.000000000000000000, 1.000000000000000000, -0.000000000000000000 ) ) ;
#836 = FACE_OUTER_BOUND ( 'NONE', #7251, .T. ) ;
#837 = CARTESIAN_POINT ( 'NONE',  ( -15.75000000000003553, -0.001000000000001000089, -2.999999999999832578 ) ) ;
#838 = CARTESIAN_POINT ( 'NONE',  ( 7.856406460551036197, 93.00000000000001421, -5.000000000000000000 ) ) ;
#839 = LINE ( 'NONE', #6642, #10047 ) ;
#840 = PRESENTATION_LAYER_ASSIGNMENT (  '', '', ( #10900 ) ) ;
#841 = ORIENTED_EDGE ( 'NONE', *, *, #5114, .F. ) ;
#842 = ORIENTED_EDGE ( 'NONE', *, *, #8332, .T. ) ;
#843 = LINE ( 'NONE', #1077, #3128 ) ;
#844 = CARTESIAN_POINT ( 'NONE',  ( 1.507608415688466075E-15, 0.4687499990440845421, -24.62111388750000174 ) ) ;
#845 = EDGE_CURVE ( 'NONE', #8849, #1367, #2420, .T. ) ;
#846 = CARTESIAN_POINT ( 'NONE',  ( -24.62111388750000174, 1.893749999044084475, -3.015216831376932151E-15 ) ) ;
#847 = CARTESIAN_POINT ( 'NONE',  ( 17.40975659021752620, 2.093749999044084653, 17.40975659021753330 ) ) ;
#848 = VECTOR ( 'NONE', #6164, 1000.000000000000000 ) ;
#849 = VERTEX_POINT ( 'NONE', #3356 ) ;
#850 = CARTESIAN_POINT ( 'NONE',  ( 0.000000000000000000, -55.00000000000000000, 0.000000000000000000 ) ) ;
#851 = DIRECTION ( 'NONE',  ( 0.000000000000000000, 0.000000000000000000, 1.000000000000000000 ) ) ;
#852 = VECTOR ( 'NONE', #9676, 1000.000000000000000 ) ;
#853 = CARTESIAN_POINT ( 'NONE',  ( -10.19839929293507552, 3.906249999044085097, 24.62111388749999463 ) ) ;
#854 = FACE_OUTER_BOUND ( 'NONE', #4694, .T. ) ;
#855 = EDGE_CURVE ( 'NONE', #3253, #7713, #7400, .T. ) ;
#856 = VERTEX_POINT ( 'NONE', #4830 ) ;
#857 = VERTEX_POINT ( 'NONE', #5867 ) ;
#858 = ORIENTED_EDGE ( 'NONE', *, *, #9260, .F. ) ;
#859 = VERTEX_POINT ( 'NONE', #787 ) ;
#860 = AXIS2_PLACEMENT_3D ( 'NONE', #2560, #5955, #5987 ) ;
#861 = ADVANCED_FACE ( 'NONE', ( #10783 ), #9999, .F. ) ;
#862 = FACE_OUTER_BOUND ( 'NONE', #9094, .T. ) ;
#863 = CARTESIAN_POINT ( 'NONE',  ( 3.058047309049977791, 19.03096903053433309, 6.296693311223928724 ) ) ;
#864 = CARTESIAN_POINT ( 'NONE',  ( 10.47307621135333200, -0.001000000000001000089, 12.13990010960489840 ) ) ;
#865 = EDGE_CURVE ( 'NONE', #4894, #10263, #9114, .T. ) ;
#866 = CYLINDRICAL_SURFACE ( 'NONE', #8002, 22.00000000000000355 ) ;
#867 = DIRECTION ( 'NONE',  ( -0.000000000000000000, -1.000000000000000000, -0.000000000000000000 ) ) ;
#868 = ADVANCED_FACE ( 'NONE', ( #9887 ), #9068, .F. ) ;
#869 = AXIS2_PLACEMENT_3D ( 'NONE', #9930, #9056, #10709 ) ;
#870 = ORIENTED_EDGE ( 'NONE', *, *, #5978, .F. ) ;
#871 = LINE ( 'NONE', #3396, #9310 ) ;
#872 = PLANE ( 'NONE',  #1414 ) ;
#873 = DIRECTION ( 'NONE',  ( -1.000000000000000000, 0.000000000000000000, 0.000000000000000000 ) ) ;
#874 = DIRECTION ( 'NONE',  ( -0.000000000000000000, -1.000000000000000000, -0.000000000000000000 ) ) ;
#875 = ORIENTED_EDGE ( 'NONE', *, *, #1882, .T. ) ;
#876 = PLANE ( 'NONE',  #6905 ) ;
#877 = ITEM_DEFINED_TRANSFORMATION ( 'NONE', 'NONE', #8444,  #7040 ) ;
#878 = CARTESIAN_POINT ( 'NONE',  ( 8.660254037844401509, 90.00000000000001421, 5.000000000000000000 ) ) ;
#879 = AXIS2_PLACEMENT_3D ( 'NONE', #8342, #7460, #2375 ) ;
#880 = VECTOR ( 'NONE', #1605, 1000.000000000000114 ) ;
#881 = DIRECTION ( 'NONE',  ( 0.000000000000000000, 1.000000000000000000, 0.000000000000000000 ) ) ;
#882 = CARTESIAN_POINT ( 'NONE',  ( 24.62111388749999108, 5.156249999044084653, 10.19839929293507730 ) ) ;
#883 = VERTEX_POINT ( 'NONE', #5047 ) ;
#884 = AXIS2_PLACEMENT_3D ( 'NONE', #2622, #6916, #2566 ) ;
#885 = VECTOR ( 'NONE', #3233, 1000.000000000000000 ) ;
#886 = CARTESIAN_POINT ( 'NONE',  ( 10.19839929293505953, 0.5812499990440845865, -24.62111388750000174 ) ) ;
#887 = CARTESIAN_POINT ( 'NONE',  ( -17.40975659021753330, 2.018749999044084475, 17.40975659021752975 ) ) ;
#888 = DIRECTION ( 'NONE',  ( -0.000000000000000000, -1.000000000000000000, -0.000000000000000000 ) ) ;
#889 = CARTESIAN_POINT ( 'NONE',  ( -25.00000000000000000, 1.112499998088169351, -3.061616997868383043E-15 ) ) ;
#890 = DIRECTION ( 'NONE',  ( -0.5000000000000073275, 0.000000000000000000, -0.8660254037844343777 ) ) ;
#891 = ORIENTED_EDGE ( 'NONE', *, *, #4982, .F. ) ;
#892 = DIRECTION ( 'NONE',  ( -1.734723475976808672E-15, 0.000000000000000000, 1.000000000000000000 ) ) ;
#893 = FILL_AREA_STYLE ('',( #59 ) ) ;
#894 = DIRECTION ( 'NONE',  ( 0.000000000000000000, -0.000000000000000000, 1.000000000000000000 ) ) ;
#895 = DIRECTION ( 'NONE',  ( -0.1767766952966370597, -0.3535533905932738419, 0.9185586535436917055 ) ) ;
#896 = DIRECTION ( 'NONE',  ( -0.000000000000000000, -1.000000000000000000, -0.000000000000000000 ) ) ;
#897 = CYLINDRICAL_SURFACE ( 'NONE', #5644, 6.999999999999997335 ) ;
#898 = AXIS2_PLACEMENT_3D ( 'NONE', #9603, #2840, #2892 ) ;
#899 = TOROIDAL_SURFACE ( 'NONE', #7083, 6.250000000000000000, 0.7500000000000000000 ) ;
#900 = ORIENTED_EDGE ( 'NONE', *, *, #1135, .T. ) ;
#901 = EDGE_LOOP ( 'NONE', ( #712, #6645, #5603, #3659 ) ) ;
#902 = ORIENTED_EDGE ( 'NONE', *, *, #7656, .F. ) ;
#903 = DIRECTION ( 'NONE',  ( 0.000000000000000000, 0.000000000000000000, 1.000000000000000000 ) ) ;
#904 = CARTESIAN_POINT ( 'NONE',  ( 24.62111388749999463, 2.331249999044084031, 10.19839929293507730 ) ) ;
#905 = LINE ( 'NONE', #10177, #2160 ) ;
#906 = CARTESIAN_POINT ( 'NONE',  ( -24.62111388750000174, 1.831249999044084475, -10.19839929293506131 ) ) ;
#907 = CARTESIAN_POINT ( 'NONE',  ( 24.99999999999999289, 0.9374999999999998890, 10.35533905932739529 ) ) ;
#908 = SURFACE_STYLE_FILL_AREA ( #4116 ) ;
#909 = ORIENTED_EDGE ( 'NONE', *, *, #4582, .F. ) ;
#910 = CARTESIAN_POINT ( 'NONE',  ( -3.500000000000049294, 20.00000000000000355, 6.062177826491040200 ) ) ;
#911 = LINE ( 'NONE', #7643, #8108 ) ;
#912 = CARTESIAN_POINT ( 'NONE',  ( 25.00000000000000000, 4.674999998088169129, -10.35533905932737753 ) ) ;
#913 = CARTESIAN_POINT ( 'NONE',  ( 1.530808498934191521E-15, 2.862499998088169573, -25.00000000000000000 ) ) ;
#914 = ORIENTED_EDGE ( 'NONE', *, *, #10318, .T. ) ;
#915 = VERTEX_POINT ( 'NONE', #4880 ) ;
#916 = EDGE_CURVE ( 'NONE', #4798, #3364, #4990, .T. ) ;
#917 = VERTEX_POINT ( 'NONE', #7517 ) ;
#918 = AXIS2_PLACEMENT_3D ( 'NONE', #5764, #9129, #6604 ) ;
#919 = EDGE_LOOP ( 'NONE', ( #68, #2381, #5556, #7537 ) ) ;
#920 = DIRECTION ( 'NONE',  ( 0.000000000000000000, 1.000000000000000000, -0.000000000000000000 ) ) ;
#921 = EDGE_CURVE ( 'NONE', #8104, #9229, #2426, .T. ) ;
#922 = DIRECTION ( 'NONE',  ( -1.000000000000000000, 0.000000000000000000, 0.000000000000000000 ) ) ;
#923 = ORIENTED_EDGE ( 'NONE', *, *, #1153, .F. ) ;
#924 = CARTESIAN_POINT ( 'NONE',  ( 10.35533905932740240, 1.812500000000000222, 24.99999999999998224 ) ) ;
#925 = CARTESIAN_POINT ( 'NONE',  ( 6.982120021884465899, 19.03096903053429401, 0.5000000000000244249 ) ) ;
#926 = CONICAL_SURFACE ( 'NONE', #3744, 4.000000000000006217, 0.1745329251994333364 ) ;
#927 = DIRECTION ( 'NONE',  ( -0.8660254037844402619, -0.4999999999999971134, 0.000000000000000000 ) ) ;
#928 = DIRECTION ( 'NONE',  ( -0.000000000000000000, 1.000000000000000000, -0.000000000000000000 ) ) ;
#929 = CARTESIAN_POINT ( 'NONE',  ( 11.57348645726024117, 5.000000000000000888, 21.83446729476942139 ) ) ;
#930 = ORIENTED_EDGE ( 'NONE', *, *, #5640, .F. ) ;
#931 = EDGE_CURVE ( 'NONE', #3835, #5793, #3995, .T. ) ;
#932 = AXIS2_PLACEMENT_3D ( 'NONE', #8431, #1760, #6794 ) ;
#933 = CIRCLE ( 'NONE', #6057, 2.999999999999997335 ) ;
#934 = ORIENTED_EDGE ( 'NONE', *, *, #377, .T. ) ;
#935 = VECTOR ( 'NONE', #8204, 1000.000000000000000 ) ;
#936 = EDGE_CURVE ( 'NONE', #10359, #5295, #2788, .T. ) ;
#937 = CARTESIAN_POINT ( 'NONE',  ( 28.02691073765301155, 94.63433907514509258, 5.000000000000000000 ) ) ;
#938 = LINE ( 'NONE', #4306, #3108 ) ;
#939 = DIRECTION ( 'NONE',  ( 0.000000000000000000, 0.000000000000000000, 1.000000000000000000 ) ) ;
#940 = AXIS2_PLACEMENT_3D ( 'NONE', #6069, #10195, #10363 ) ;
#941 = CARTESIAN_POINT ( 'NONE',  ( -15.60400172474278158, 28.00000000000000000, -12.47307621135316680 ) ) ;
#942 = ITEM_DEFINED_TRANSFORMATION ( 'NONE', 'NONE', #9855,  #7040 ) ;
#943 = CIRCLE ( 'NONE', #10817, 2.149999999999999911 ) ;
#944 = DIRECTION ( 'NONE',  ( -0.000000000000000000, -0.000000000000000000, 1.000000000000000000 ) ) ;
#945 = CARTESIAN_POINT ( 'NONE',  ( 14.00000000000000533, 0.000000000000000000, 2.000000000000004441 ) ) ;
#946 = CARTESIAN_POINT ( 'NONE',  ( 1.507608415688466075E-15, 4.468749999044084653, -24.62111388750000174 ) ) ;
#947 = AXIS2_PLACEMENT_3D ( 'NONE', #8244, #10531, #8975 ) ;
#948 = CIRCLE ( 'NONE', #4114, 5.750000000000006217 ) ;
#949 = EDGE_CURVE ( 'NONE', #3818, #3051, #10896, .T. ) ;
#950 = CARTESIAN_POINT ( 'NONE',  ( 24.62111388750000174, 1.393749999044084475, 0.000000000000000000 ) ) ;
#951 = CARTESIAN_POINT ( 'NONE',  ( 10.19839929293505953, 1.581249999044084475, -24.62111388750000174 ) ) ;
#952 = CARTESIAN_POINT ( 'NONE',  ( 17.67766952966368521, 1.875000000000000000, 17.67766952966369232 ) ) ;
#953 = AXIS2_PLACEMENT_3D ( 'NONE', #6193, #7077, #10436 ) ;
#954 = CARTESIAN_POINT ( 'NONE',  ( 10.19839929293506486, 5.031249999044083765, 24.62111388749999819 ) ) ;
#955 = CARTESIAN_POINT ( 'NONE',  ( 28.89716436598705585, 102.6833647615033840, -5.000000000000000000 ) ) ;
#956 = VERTEX_POINT ( 'NONE', #4935 ) ;
#957 = LINE ( 'NONE', #9457, #7069 ) ;
#958 =( NAMED_UNIT ( * ) PLANE_ANGLE_UNIT ( ) SI_UNIT ( $, .RADIAN. ) );
#959 = CYLINDRICAL_SURFACE ( 'NONE', #3390, 6.000000000000000888 ) ;
#960 = CARTESIAN_POINT ( 'NONE',  ( -25.00000000000000000, 2.049999998088169129, -10.35533905932738108 ) ) ;
#961 = CARTESIAN_POINT ( 'NONE',  ( 0.000000000000000000, 28.00000000000000000, -7.500000000000000888 ) ) ;
#962 = CARTESIAN_POINT ( 'NONE',  ( 17.67766952966369232, 4.125000000000000000, -17.67766952966369232 ) ) ;
#963 = VERTEX_POINT ( 'NONE', #10056 ) ;
#964 = VECTOR ( 'NONE', #1264, 1000.000000000000000 ) ;
#965 = EDGE_LOOP ( 'NONE', ( #9121, #8922, #199, #5165 ) ) ;
#966 = ORIENTED_EDGE ( 'NONE', *, *, #8610, .T. ) ;
#967 = ORIENTED_EDGE ( 'NONE', *, *, #2281, .F. ) ;
#968 = CARTESIAN_POINT ( 'NONE',  ( 3.957930336368489021E-15, 28.00000000000000000, 19.75000000000000000 ) ) ;
#969 = CARTESIAN_POINT ( 'NONE',  ( 10.19839929293505953, 4.581249999044085364, -24.62111388750000174 ) ) ;
#970 = CARTESIAN_POINT ( 'NONE',  ( 1.507608415688466075E-15, 0.6437499990440845865, -24.62111388750000174 ) ) ;
#971 = CARTESIAN_POINT ( 'NONE',  ( 17.40975659021752620, 1.268749999044084475, 17.40975659021753330 ) ) ;
#972 = CARTESIAN_POINT ( 'NONE',  ( -24.62111388750000884, 2.781249999044085541, 10.19839929293505421 ) ) ;
#973 = FACE_OUTER_BOUND ( 'NONE', #9739, .T. ) ;
#974 = FACE_BOUND ( 'NONE', #8390, .T. ) ;
#975 = CYLINDRICAL_SURFACE ( 'NONE', #2480, 25.00000000000000000 ) ;
#976 = LINE ( 'NONE', #2030, #752 ) ;
#977 = ORIENTED_EDGE ( 'NONE', *, *, #1807, .T. ) ;
#978 = VERTEX_POINT ( 'NONE', #1668 ) ;
#979 = CARTESIAN_POINT ( 'NONE',  ( 0.000000000000000000, 10.00000000000000355, 0.000000000000000000 ) ) ;
#980 = DIRECTION ( 'NONE',  ( 0.000000000000000000, -1.000000000000000000, 0.000000000000000000 ) ) ;
#981 = ORIENTED_EDGE ( 'NONE', *, *, #5799, .F. ) ;
#982 = CARTESIAN_POINT ( 'NONE',  ( 1.500000000000001332, 0.000000000000000000, 0.000000000000000000 ) ) ;
#983 = CARTESIAN_POINT ( 'NONE',  ( 0.000000000000000000, 20.00000000000000355, 20.00000000000000000 ) ) ;
#984 =( BOUNDED_CURVE ( )  B_SPLINE_CURVE ( 3, ( #8489, #6736, #6844, #2563 ),
 .UNSPECIFIED., .F., .T. ) 
 B_SPLINE_CURVE_WITH_KNOTS ( ( 4, 4 ),
 ( 3.927175151554402888, 3.998664601439924304 ),
 .UNSPECIFIED. ) 
 CURVE ( )  GEOMETRIC_REPRESENTATION_ITEM ( )  RATIONAL_B_SPLINE_CURVE ( ( 1.000000000000000000, 0.9995741502243209453, 0.9995741502243209453, 1.000000000000000000 ) ) 
 REPRESENTATION_ITEM ( '' )  );
#985 = DIRECTION ( 'NONE',  ( 0.000000000000000000, 0.000000000000000000, -1.000000000000000000 ) ) ;
#986 = LINE ( 'NONE', #9545, #1256 ) ;
#987 = DIRECTION ( 'NONE',  ( -0.4330127018922191318, 0.8660254037844380415, -0.2500000000000026090 ) ) ;
#988 = DIRECTION ( 'NONE',  ( 0.4999999999999980016, 0.000000000000000000, 0.8660254037844398178 ) ) ;
#989 = ORIENTED_EDGE ( 'NONE', *, *, #1979, .F. ) ;
#990 = ORIENTED_EDGE ( 'NONE', *, *, #7446, .T. ) ;
#991 = PLANE ( 'NONE',  #10921 ) ;
#992 = LINE ( 'NONE', #3335, #8666 ) ;
#993 = CARTESIAN_POINT ( 'NONE',  ( -10.35533905932737575, 3.924999998088168685, -25.00000000000000000 ) ) ;
#994 = EDGE_CURVE ( 'NONE', #9664, #5784, #7058, .T. ) ;
#995 = CARTESIAN_POINT ( 'NONE',  ( -10.19839929293507375, 4.081249999044084475, 24.62111388749999108 ) ) ;
#996 = ORIENTED_EDGE ( 'NONE', *, *, #453, .F. ) ;
#997 = EDGE_CURVE ( 'NONE', #6764, #7282, #10390, .T. ) ;
#998 = DIRECTION ( 'NONE',  ( 0.5000000000000009992, 0.000000000000000000, 0.8660254037844380415 ) ) ;
#999 = DIRECTION ( 'NONE',  ( 0.000000000000000000, -1.000000000000000000, 0.000000000000000000 ) ) ;
#1000 = CARTESIAN_POINT ( 'NONE',  ( 1.500000000000000000, 83.00000000000000000, 1.500000000000000000 ) ) ;
#1001 = ADVANCED_FACE ( 'NONE', ( #1013 ), #7805, .F. ) ;
#1002 = ORIENTED_EDGE ( 'NONE', *, *, #1471, .T. ) ;
#1003 = CARTESIAN_POINT ( 'NONE',  ( -17.40975659021752975, 1.768749999044084475, -17.40975659021752975 ) ) ;
#1004 = CARTESIAN_POINT ( 'NONE',  ( -11.06217782649114412, 10.00000000000000533, 6.386751345948026071 ) ) ;
#1005 = CARTESIAN_POINT ( 'NONE',  ( 25.00000000000000000, 3.062500000000000000, -10.35533905932737753 ) ) ;
#1006 = DIRECTION ( 'NONE',  ( 0.000000000000000000, 1.000000000000000000, 0.000000000000000000 ) ) ;
#1007 = ORIENTED_EDGE ( 'NONE', *, *, #4743, .T. ) ;
#1008 = EDGE_CURVE ( 'NONE', #9883, #7303, #1839, .T. ) ;
#1009 = DIRECTION ( 'NONE',  ( -0.8660254037844328234, 0.000000000000000000, 0.5000000000000098810 ) ) ;
#1010 = SHAPE_REPRESENTATION_RELATIONSHIP ( 'NONE' , 'NONE' ,  #7612, #4934 ) ;
#1011 = DIRECTION ( 'NONE',  ( -0.4999999999999888978, 0.000000000000000000, 0.8660254037844450359 ) ) ;
#1012 = FACE_BOUND ( 'NONE', #6871, .T. ) ;
#1013 = FACE_OUTER_BOUND ( 'NONE', #2172, .T. ) ;
#1014 = DIRECTION ( 'NONE',  ( -0.000000000000000000, 1.000000000000000000, -0.000000000000000000 ) ) ;
#1015 = CARTESIAN_POINT ( 'NONE',  ( 24.99999999999999289, 3.937500000000000000, 10.35533905932739529 ) ) ;
#1016 = EDGE_CURVE ( 'NONE', #8941, #10020, #1128, .T. ) ;
#1017 = ORIENTED_EDGE ( 'NONE', *, *, #3787, .T. ) ;
#1018 = EDGE_LOOP ( 'NONE', ( #3836, #1523 ) ) ;
#1019 =( GEOMETRIC_REPRESENTATION_CONTEXT ( 3 ) GLOBAL_UNCERTAINTY_ASSIGNED_CONTEXT ( ( #1395 ) ) GLOBAL_UNIT_ASSIGNED_CONTEXT ( ( #2530, #3296, #4932 ) ) REPRESENTATION_CONTEXT ( 'NONE', 'WORKASPACE' ) );
#1020 = CARTESIAN_POINT ( 'NONE',  ( 9.184850993605149917E-16, 31.00000000000000000, 7.500000000000000888 ) ) ;
#1021 = CARTESIAN_POINT ( 'NONE',  ( -24.62111388750000174, 3.893749999044084475, -3.015216831376932151E-15 ) ) ;
#1022 = DIRECTION ( 'NONE',  ( 0.000000000000000000, 1.000000000000000000, 0.000000000000000000 ) ) ;
#1023 = CARTESIAN_POINT ( 'NONE',  ( 17.67766952966369232, 4.737499998088169129, -17.67766952966369232 ) ) ;
#1024 = CARTESIAN_POINT ( 'NONE',  ( -17.40975659021753330, 4.843749999044083765, 17.40975659021752975 ) ) ;
#1025 = DIRECTION ( 'NONE',  ( 0.000000000000000000, 0.000000000000000000, 1.000000000000000000 ) ) ;
#1026 = CARTESIAN_POINT ( 'NONE',  ( -5.890223162633902554, 19.34316356887877220, 3.785909150702991166 ) ) ;
#1027 = DIRECTION ( 'NONE',  ( 0.000000000000000000, -1.000000000000000000, 0.000000000000000000 ) ) ;
#1028 = FACE_OUTER_BOUND ( 'NONE', #4958, .T. ) ;
#1029 = STYLED_ITEM ( 'NONE', ( #4490 ), #10733 ) ;
#1030 = CARTESIAN_POINT ( 'NONE',  ( 17.40975659021752975, 4.343749999044084653, -17.40975659021752975 ) ) ;
#1031 = DIRECTION ( 'NONE',  ( 0.9659258262890684232, -0.2588190451025202399, 0.000000000000000000 ) ) ;
#1032 = EDGE_LOOP ( 'NONE', ( #3309, #9854, #6146, #10751, #8965, #2173 ) ) ;
#1033 = EDGE_LOOP ( 'NONE', ( #9297, #6954, #9499, #8643 ) ) ;
#1034 = ORIENTED_EDGE ( 'NONE', *, *, #10874, .F. ) ;
#1035 = DIRECTION ( 'NONE',  ( 0.000000000000000000, 1.000000000000000000, 0.000000000000000000 ) ) ;
#1036 =( GEOMETRIC_REPRESENTATION_CONTEXT ( 3 ) GLOBAL_UNCERTAINTY_ASSIGNED_CONTEXT ( ( #3144 ) ) GLOBAL_UNIT_ASSIGNED_CONTEXT ( ( #2061, #10617, #3724 ) ) REPRESENTATION_CONTEXT ( 'NONE', 'WORKASPACE' ) );
#1037 = VECTOR ( 'NONE', #2963, 1000.000000000000000 ) ;
#1038 = PLANE ( 'NONE',  #2001 ) ;
#1039 = EDGE_LOOP ( 'NONE', ( #7017, #6117, #1492, #5769 ) ) ;
#1040 = DIRECTION ( 'NONE',  ( -0.000000000000000000, -1.000000000000000000, -0.000000000000000000 ) ) ;
#1041 = DIRECTION ( 'NONE',  ( 0.2588190451025202399, 0.9659258262890684232, -0.000000000000000000 ) ) ;
#1042 = CARTESIAN_POINT ( 'NONE',  ( -7.875000000000116351, 25.00000000000000000, -13.63990010960484334 ) ) ;
#1043 = DIRECTION ( 'NONE',  ( -0.2499999999999980016, 0.8660254037844380415, -0.4330127018922217408 ) ) ;
#1044 = FACE_OUTER_BOUND ( 'NONE', #8271, .T. ) ;
#1045 = CARTESIAN_POINT ( 'NONE',  ( 0.000000000000000000, 83.00000000000000000, 0.000000000000000000 ) ) ;
#1046 = APPLICATION_CONTEXT ( 'automotive_design' ) ;
#1047 = AXIS2_PLACEMENT_3D ( 'NONE', #1899, #5280, #4212 ) ;
#1048 = PRODUCT_RELATED_PRODUCT_CATEGORY ( 'part', '', ( #361 ) ) ;
#1049 = ORIENTED_EDGE ( 'NONE', *, *, #196, .T. ) ;
#1050 = CARTESIAN_POINT ( 'NONE',  ( -4.592425496802574367E-15, 5.362499998088169129, 25.00000000000000000 ) ) ;
#1051 = CARTESIAN_POINT ( 'NONE',  ( -4.522825247065398226E-15, 1.143749999044084475, 24.62111388750000174 ) ) ;
#1052 =( BOUNDED_CURVE ( )  B_SPLINE_CURVE ( 2, ( #2193, #5570, #7270, #10650, #3059, #6455, #2236, #1412, #4073 ),
 .UNSPECIFIED., .F., .F. ) 
 B_SPLINE_CURVE_WITH_KNOTS ( ( 3, 2, 2, 2, 3 ),
 ( 0.7500000000000000000, 0.7750000000000000222, 0.8000000000000000444, 0.8250000000000000666, 0.8500000000000000888 ),
 .UNSPECIFIED. ) 
 CURVE ( )  GEOMETRIC_REPRESENTATION_ITEM ( )  RATIONAL_B_SPLINE_CURVE ( ( 1.000000000000000000, 0.9238795325112867385, 1.000000000000000000, 0.9238795325112867385, 1.000000000000000000, 0.9238795325112867385, 1.000000000000000000, 0.9238795325112864054, 1.000000000000000444 ) ) 
 REPRESENTATION_ITEM ( '' )  );
#1053 = LINE ( 'NONE', #4308, #3154 ) ;
#1054 = APPLICATION_PROTOCOL_DEFINITION ( 'draft international standard', 'automotive_design', 1998, #3263 ) ;
#1055 = LINE ( 'NONE', #10332, #4311 ) ;
#1056 = DIRECTION ( 'NONE',  ( -0.000000000000000000, -1.000000000000000000, -0.000000000000000000 ) ) ;
#1057 = CARTESIAN_POINT ( 'NONE',  ( 17.40975659021752975, 4.343749999044084653, -17.40975659021752975 ) ) ;
#1058 = ADVANCED_FACE ( 'NONE', ( #4325 ), #4262, .T. ) ;
#1059 = CARTESIAN_POINT ( 'NONE',  ( -10.19839929293505776, 1.706249999044084698, -24.62111388750000174 ) ) ;
#1060 = CARTESIAN_POINT ( 'NONE',  ( -10.19839929293507552, 4.081249999044084475, 24.62111388749999463 ) ) ;
#1061 = DIRECTION ( 'NONE',  ( 1.000000000000000000, 0.000000000000000000, 0.000000000000000000 ) ) ;
#1062 = LINE ( 'NONE', #7619, #7030 ) ;
#1063 = DIRECTION ( 'NONE',  ( 1.000000000000000000, 0.000000000000000000, 0.000000000000000000 ) ) ;
#1064 = VERTEX_POINT ( 'NONE', #4444 ) ;
#1065 = FACE_OUTER_BOUND ( 'NONE', #3101, .T. ) ;
#1066 = EDGE_CURVE ( 'NONE', #241, #6044, #675, .T. ) ;
#1067 = PLANE ( 'NONE',  #8873 ) ;
#1068 = DIRECTION ( 'NONE',  ( 0.000000000000000000, 0.000000000000000000, -1.000000000000000000 ) ) ;
#1069 = DIRECTION ( 'NONE',  ( 0.5000000000000009992, 0.000000000000000000, -0.8660254037844380415 ) ) ;
#1070 = CARTESIAN_POINT ( 'NONE',  ( 10.35533905932737930, 3.187500000000000000, -25.00000000000000000 ) ) ;
#1071 = AXIS2_PLACEMENT_3D ( 'NONE', #8171, #7438, #3226 ) ;
#1072 = EDGE_LOOP ( 'NONE', ( #5589, #3090, #10487, #3502 ) ) ;
#1073 = AXIS2_PLACEMENT_3D ( 'NONE', #10856, #9237, #8408 ) ;
#1074 = ORIENTED_EDGE ( 'NONE', *, *, #3776, .T. ) ;
#1075 = EDGE_CURVE ( 'NONE', #9988, #3378, #10729, .T. ) ;
#1076 = ORIENTED_EDGE ( 'NONE', *, *, #4297, .F. ) ;
#1077 = CARTESIAN_POINT ( 'NONE',  ( -15.74999999999997158, -0.001000000000001000089, 3.000000000000165645 ) ) ;
#1078 = CARTESIAN_POINT ( 'NONE',  ( -17.40975659021753330, 5.018749999044084475, 17.40975659021752975 ) ) ;
#1079 = LINE ( 'NONE', #10349, #6951 ) ;
#1080 = CARTESIAN_POINT ( 'NONE',  ( -25.00000000000001421, 4.174999998088169129, 10.35533905932737397 ) ) ;
#1081 = CARTESIAN_POINT ( 'NONE',  ( -24.62111388750000884, 4.781249999044083765, 10.19839929293505421 ) ) ;
#1082 = ADVANCED_FACE ( 'NONE', ( #10116 ), #9716, .T. ) ;
#1083 = VECTOR ( 'NONE', #8766, 1000.000000000000000 ) ;
#1084 = TOROIDAL_SURFACE ( 'NONE', #7782, 7.399999999999999467, 0.1000000000000000472 ) ;
#1085 = DIRECTION ( 'NONE',  ( 0.000000000000000000, 2.775557561562888270E-17, 1.000000000000000000 ) ) ;
#1086 = DIRECTION ( 'NONE',  ( 0.000000000000000000, -1.000000000000000000, 0.000000000000000000 ) ) ;
#1087 = LINE ( 'NONE', #7821, #4265 ) ;
#1088 = DIRECTION ( 'NONE',  ( 0.000000000000000000, 0.000000000000000000, 1.000000000000000000 ) ) ;
#1089 = CARTESIAN_POINT ( 'NONE',  ( -10.19839929293507552, 4.906249999044083765, 24.62111388749999463 ) ) ;
#1090 = CARTESIAN_POINT ( 'NONE',  ( 3.050810944027392283E-15, -8.528980942125404141, 24.91176187412963117 ) ) ;
#1091 = ORIENTED_EDGE ( 'NONE', *, *, #2592, .F. ) ;
#1092 = ORIENTED_EDGE ( 'NONE', *, *, #10848, .F. ) ;
#1093 = ORIENTED_EDGE ( 'NONE', *, *, #10175, .T. ) ;
#1094 = AXIS2_PLACEMENT_3D ( 'NONE', #5441, #5400, #9532 ) ;
#1095 = CARTESIAN_POINT ( 'NONE',  ( 2.999999999999997335, 28.00000000000000000, -15.75000000000000355 ) ) ;
#1096 = EDGE_CURVE ( 'NONE', #8849, #8924, #1941, .T. ) ;
#1097 = DIRECTION ( 'NONE',  ( 0.000000000000000000, -1.000000000000000000, 0.000000000000000000 ) ) ;
#1098 = CARTESIAN_POINT ( 'NONE',  ( -4.592425496802574367E-15, 2.750000000000000000, 25.00000000000000000 ) ) ;
#1099 = FACE_OUTER_BOUND ( 'NONE', #4676, .T. ) ;
#1100 = DIRECTION ( 'NONE',  ( -0.000000000000000000, -1.000000000000000000, -0.000000000000000000 ) ) ;
#1101 = CARTESIAN_POINT ( 'NONE',  ( 0.000000000000000000, 7.000000000000003553, 0.000000000000000000 ) ) ;
#1102 = FACE_OUTER_BOUND ( 'NONE', #9137, .T. ) ;
#1103 = CARTESIAN_POINT ( 'NONE',  ( 24.62111388749999463, 4.331249999044084475, 10.19839929293507730 ) ) ;
#1104 = VECTOR ( 'NONE', #7309, 999.9999999999998863 ) ;
#1105 = ORIENTED_EDGE ( 'NONE', *, *, #4602, .T. ) ;
#1106 = ORIENTED_EDGE ( 'NONE', *, *, #4297, .T. ) ;
#1107 = CARTESIAN_POINT ( 'NONE',  ( 0.5000000000000000000, 0.000000000000000000, 0.000000000000000000 ) ) ;
#1108 = CARTESIAN_POINT ( 'NONE',  ( 25.00000000000000000, 1.674999998088169351, -10.35533905932737753 ) ) ;
#1109 = CIRCLE ( 'NONE', #2847, 6.999999999999997335 ) ;
#1110 = CARTESIAN_POINT ( 'NONE',  ( -17.40975659021752975, 3.768749999044084475, -17.40975659021752975 ) ) ;
#1111 = ORIENTED_EDGE ( 'NONE', *, *, #7014, .F. ) ;
#1112 = CARTESIAN_POINT ( 'NONE',  ( 5.796693311223892309, 19.03096903053431532, 3.924072712834481447 ) ) ;
#1113 = FACE_OUTER_BOUND ( 'NONE', #1896, .T. ) ;
#1114 = CARTESIAN_POINT ( 'NONE',  ( 0.000000000000000000, 85.00000000000000000, -25.00000000000000000 ) ) ;
#1115 = CARTESIAN_POINT ( 'NONE',  ( -5.000000000000000000, 90.00000000000001421, 0.000000000000000000 ) ) ;
#1116 = VECTOR ( 'NONE', #5042, 1000.000000000000227 ) ;
#1117 =( BOUNDED_CURVE ( )  B_SPLINE_CURVE ( 3, ( #5452, #2124, #8041, #4691 ),
 .UNSPECIFIED., .F., .F. ) 
 B_SPLINE_CURVE_WITH_KNOTS ( ( 4, 4 ),
 ( 3.927175151554401999, 3.998664601439922972 ),
 .UNSPECIFIED. ) 
 CURVE ( )  GEOMETRIC_REPRESENTATION_ITEM ( )  RATIONAL_B_SPLINE_CURVE ( ( 1.000000000000000000, 0.9995741502243209453, 0.9995741502243209453, 1.000000000000000000 ) ) 
 REPRESENTATION_ITEM ( '' )  );
#1118 = AXIS2_PLACEMENT_3D ( 'NONE', #8201, #3910, #5621 ) ;
#1119 = FACE_OUTER_BOUND ( 'NONE', #5894, .T. ) ;
#1120 = CARTESIAN_POINT ( 'NONE',  ( -10.35533905932737575, 0.9249999980881692396, -25.00000000000000000 ) ) ;
#1121 = DIRECTION ( 'NONE',  ( 0.000000000000000000, 1.000000000000000000, -0.000000000000000000 ) ) ;
#1122 = ORIENTED_EDGE ( 'NONE', *, *, #3481, .F. ) ;
#1123 = DIRECTION ( 'NONE',  ( 1.000000000000000000, 0.000000000000000000, -0.000000000000000000 ) ) ;
#1124 = DIRECTION ( 'NONE',  ( 0.000000000000000000, 0.000000000000000000, -1.000000000000000000 ) ) ;
#1125 = VECTOR ( 'NONE', #3487, 1000.000000000000000 ) ;
#1126 = CARTESIAN_POINT ( 'NONE',  ( -24.62111388750000174, 0.7187499990440845421, -3.015216831376932151E-15 ) ) ;
#1127 = EDGE_CURVE ( 'NONE', #6508, #3052, #9847, .T. ) ;
#1128 = LINE ( 'NONE', #10289, #4919 ) ;
#1129 = EDGE_CURVE ( 'NONE', #9174, #2551, #4750, .T. ) ;
#1130 = ORIENTED_EDGE ( 'NONE', *, *, #1287, .T. ) ;
#1131 = CIRCLE ( 'NONE', #9596, 25.00000000000000000 ) ;
#1132 = ORIENTED_EDGE ( 'NONE', *, *, #9956, .T. ) ;
#1133 = VERTEX_POINT ( 'NONE', #6203 ) ;
#1134 = EDGE_LOOP ( 'NONE', ( #1798, #4684, #4225, #996 ) ) ;
#1135 = EDGE_CURVE ( 'NONE', #6439, #7005, #598, .T. ) ;
#1136 = AXIS2_PLACEMENT_3D ( 'NONE', #9771, #8895, #5691 ) ;
#1137 = CARTESIAN_POINT ( 'NONE',  ( 0.000000000000000000, 10.00000000000000355, 0.000000000000000000 ) ) ;
#1138 = CARTESIAN_POINT ( 'NONE',  ( -24.62111388750000884, 1.781249999044084431, 10.19839929293505421 ) ) ;
#1139 = CARTESIAN_POINT ( 'NONE',  ( 25.00000000000000000, 0.6749999980881691286, -10.35533905932737753 ) ) ;
#1140 = CARTESIAN_POINT ( 'NONE',  ( 10.35533905932738286, 3.424999998088169573, 24.99999999999999645 ) ) ;
#1141 = AXIS2_PLACEMENT_3D ( 'NONE', #1158, #7987, #9693 ) ;
#1142 = CARTESIAN_POINT ( 'NONE',  ( 24.62111388750000174, 4.218749999044084653, 0.000000000000000000 ) ) ;
#1143 = ADVANCED_FACE ( 'NONE', ( #648 ), #10756, .F. ) ;
#1144 = EDGE_CURVE ( 'NONE', #4659, #9481, #7929, .T. ) ;
#1145 = CARTESIAN_POINT ( 'NONE',  ( 3.355508642977490297, 19.66631150450992749, -6.145599950363587638 ) ) ;
#1146 = PLANE ( 'NONE',  #1766 ) ;
#1147 = EDGE_CURVE ( 'NONE', #10413, #5164, #4139, .T. ) ;
#1148 = CARTESIAN_POINT ( 'NONE',  ( 1.530808498934191521E-15, 2.250000000000000444, -25.00000000000000000 ) ) ;
#1149 = CARTESIAN_POINT ( 'NONE',  ( -4.592425496802574367E-15, 4.750000000000000000, 25.00000000000000000 ) ) ;
#1150 = AXIS2_PLACEMENT_3D ( 'NONE', #9805, #4699, #8881 ) ;
#1151 = CARTESIAN_POINT ( 'NONE',  ( -17.67766952966368876, 2.375000000000000000, -17.67766952966369232 ) ) ;
#1152 = DIRECTION ( 'NONE',  ( 0.000000000000000000, 0.000000000000000000, -1.000000000000000000 ) ) ;
#1153 = EDGE_CURVE ( 'NONE', #7275, #5714, #1385, .T. ) ;
#1154 = CARTESIAN_POINT ( 'NONE',  ( -12.69999999999998153, 2.449293598294711838E-16, -2.000000000000004441 ) ) ;
#1155 = CARTESIAN_POINT ( 'NONE',  ( 11.92163336986827815, 7.781088913245563177, 6.305607966083920601 ) ) ;
#1156 = ORIENTED_EDGE ( 'NONE', *, *, #1512, .F. ) ;
#1157 = EDGE_CURVE ( 'NONE', #7830, #2468, #8435, .T. ) ;
#1158 = CARTESIAN_POINT ( 'NONE',  ( -0.1920286436967143240, 0.000000000000000000, 0.000000000000000000 ) ) ;
#1159 = DIRECTION ( 'NONE',  ( 0.000000000000000000, 1.000000000000000000, 0.000000000000000000 ) ) ;
#1160 = DIRECTION ( 'NONE',  ( 0.000000000000000000, 0.000000000000000000, 1.000000000000000000 ) ) ;
#1161 = CYLINDRICAL_SURFACE ( 'NONE', #5135, 2.000000000000000000 ) ;
#1162 = CARTESIAN_POINT ( 'NONE',  ( -25.00000000000000000, 1.500000000000000000, -3.061616997868383043E-15 ) ) ;
#1163 = DIRECTION ( 'NONE',  ( 0.000000000000000000, 0.000000000000000000, 1.000000000000000000 ) ) ;
#1164 = ORIENTED_EDGE ( 'NONE', *, *, #4969, .T. ) ;
#1165 = ORIENTED_EDGE ( 'NONE', *, *, #6990, .F. ) ;
#1166 = EDGE_CURVE ( 'NONE', #5553, #2933, #871, .T. ) ;
#1167 = EDGE_LOOP ( 'NONE', ( #7022, #430, #3791, #5634, #3288, #6183 ) ) ;
#1168 = CARTESIAN_POINT ( 'NONE',  ( 25.00000000000000000, 1.612499998088169351, 0.000000000000000000 ) ) ;
#1169 = CARTESIAN_POINT ( 'NONE',  ( 24.62111388750000174, 1.456249999044084920, -10.19839929293505776 ) ) ;
#1170 = DIRECTION ( 'NONE',  ( -0.000000000000000000, -1.000000000000000000, -0.000000000000000000 ) ) ;
#1171 = PLANE ( 'NONE',  #8884 ) ;
#1172 = DIRECTION ( 'NONE',  ( 0.000000000000000000, -1.000000000000000000, 0.000000000000000000 ) ) ;
#1173 = ORIENTED_EDGE ( 'NONE', *, *, #4852, .F. ) ;
#1174 = CARTESIAN_POINT ( 'NONE',  ( -24.62111388750000174, 4.893749999044084475, -3.015216831376932151E-15 ) ) ;
#1175 = CARTESIAN_POINT ( 'NONE',  ( 6.982120021884465899, 10.00000000000000355, 0.5000000000000244249 ) ) ;
#1176 = CARTESIAN_POINT ( 'NONE',  ( -20.77469822633729279, 4.999999999999997335, -13.92348360573865840 ) ) ;
#1177 = FACE_BOUND ( 'NONE', #4966, .T. ) ;
#1178 = ORIENTED_EDGE ( 'NONE', *, *, #2398, .T. ) ;
#1179 = CARTESIAN_POINT ( 'NONE',  ( 67.07963283087528339, 92.45240317130979690, 5.000000000000000000 ) ) ;
#1180 = CARTESIAN_POINT ( 'NONE',  ( 0.000000000000000000, 85.00000000000000000, -28.00000000000000000 ) ) ;
#1181 = CARTESIAN_POINT ( 'NONE',  ( 10.19839929293505953, 4.406249999044084653, -24.62111388750000174 ) ) ;
#1182 = DIRECTION ( 'NONE',  ( 0.5000000000000073275, 0.000000000000000000, 0.8660254037844343777 ) ) ;
#1183 = ORIENTED_EDGE ( 'NONE', *, *, #8064, .F. ) ;
#1184 = ORIENTED_EDGE ( 'NONE', *, *, #1672, .F. ) ;
#1185 = DIRECTION ( 'NONE',  ( 0.4330127018922207971, -0.8660254037844380415, -0.2499999999999995004 ) ) ;
#1186 = CARTESIAN_POINT ( 'NONE',  ( 24.62111388750000174, 4.281249999044084653, -10.19839929293505776 ) ) ;
#1187 = CARTESIAN_POINT ( 'NONE',  ( 17.40975659021752975, 4.518749999044085364, -17.40975659021752975 ) ) ;
#1188 = CARTESIAN_POINT ( 'NONE',  ( -25.00000000000000000, 4.112499998088169129, -3.061616997868383043E-15 ) ) ;
#1189 = CARTESIAN_POINT ( 'NONE',  ( -17.67766952966369232, 3.625000000000000000, 17.67766952966368876 ) ) ;
#1190 = CARTESIAN_POINT ( 'NONE',  ( 25.00000000000000000, 8.000000000000003553, 0.000000000000000000 ) ) ;
#1191 = CARTESIAN_POINT ( 'NONE',  ( -20.63749999999999929, 0.000000000000000000, 0.000000000000000000 ) ) ;
#1192 = DIRECTION ( 'NONE',  ( -0.8660254037844382635, -0.5000000000000004441, 0.000000000000000000 ) ) ;
#1193 = DIRECTION ( 'NONE',  ( -0.8660254037844362651, 0.000000000000000000, 0.5000000000000042188 ) ) ;
#1194 = LINE ( 'NONE', #8583, #1830 ) ;
#1195 = ORIENTED_EDGE ( 'NONE', *, *, #9439, .F. ) ;
#1196 = EDGE_LOOP ( 'NONE', ( #731, #8937, #10125 ) ) ;
#1197 = EDGE_CURVE ( 'NONE', #9938, #6120, #10204, .T. ) ;
#1198 = ORIENTED_EDGE ( 'NONE', *, *, #94, .T. ) ;
#1199 = EDGE_CURVE ( 'NONE', #10020, #10364, #1818, .T. ) ;
#1200 = CARTESIAN_POINT ( 'NONE',  ( 3.050810944027392283E-15, -55.00000000000000000, 24.91176187412963117 ) ) ;
#1201 = CARTESIAN_POINT ( 'NONE',  ( -10.35533905932737575, 3.924999998088168685, -25.00000000000000000 ) ) ;
#1202 = DIRECTION ( 'NONE',  ( 0.000000000000000000, 0.000000000000000000, 1.000000000000000000 ) ) ;
#1203 = EDGE_CURVE ( 'NONE', #9038, #4797, #2952, .T. ) ;
#1204 = CARTESIAN_POINT ( 'NONE',  ( 17.10400172474269098, 25.00000000000000000, 9.874999999999957367 ) ) ;
#1205 = AXIS2_PLACEMENT_3D ( 'NONE', #2985, #7162, #9742 ) ;
#1206 = CARTESIAN_POINT ( 'NONE',  ( -3.058047309049933382, 19.03096903053431532, -6.296693311223948264 ) ) ;
#1207 = DIRECTION ( 'NONE',  ( -1.000000000000000000, 0.000000000000000000, 0.000000000000000000 ) ) ;
#1208 = CARTESIAN_POINT ( 'NONE',  ( -10.19839929293505776, 3.706249999044084920, -24.62111388750000174 ) ) ;
#1209 = AXIS2_PLACEMENT_3D ( 'NONE', #6734, #5206, #8547 ) ;
#1210 = ADVANCED_FACE ( 'NONE', ( #5028, #820 ), #991, .T. ) ;
#1211 = EDGE_LOOP ( 'NONE', ( #2757, #9774 ) ) ;
#1212 = AXIS2_PLACEMENT_3D ( 'NONE', #668, #8227, #10723 ) ;
#1213 = EDGE_CURVE ( 'NONE', #1851, #7784, #154, .T. ) ;
#1214 = CARTESIAN_POINT ( 'NONE',  ( -10.19839929293505776, 2.706249999044084475, -24.62111388750000174 ) ) ;
#1215 = CARTESIAN_POINT ( 'NONE',  ( 0.000000000000000000, 85.00000000000000000, 0.000000000000000000 ) ) ;
#1216 = EDGE_CURVE ( 'NONE', #2617, #9902, #2682, .T. ) ;
#1217 = DIRECTION ( 'NONE',  ( 0.000000000000000000, 0.000000000000000000, -1.000000000000000000 ) ) ;
#1218 = AXIS2_PLACEMENT_3D ( 'NONE', #4887, #10853, #1618 ) ;
#1219 = DIRECTION ( 'NONE',  ( 0.000000000000000000, 1.000000000000000000, -0.000000000000000000 ) ) ;
#1220 = CARTESIAN_POINT ( 'NONE',  ( -1.500000000000000444, 83.00000000000000000, -1.500000000000000222 ) ) ;
#1221 = AXIS2_PLACEMENT_3D ( 'NONE', #4453, #8456, #2645 ) ;
#1222 = EDGE_LOOP ( 'NONE', ( #9049, #9429 ) ) ;
#1223 = LINE ( 'NONE', #1175, #1967 ) ;
#1224 = CARTESIAN_POINT ( 'NONE',  ( -24.71676035596633270, 5.000000000000000000, 2.273299333383253185 ) ) ;
#1225 = CARTESIAN_POINT ( 'NONE',  ( 17.40975659021752975, 0.5187499990440845865, -17.40975659021752975 ) ) ;
#1226 = ADVANCED_FACE ( 'NONE', ( #10148 ), #2458, .T. ) ;
#1227 = VERTEX_POINT ( 'NONE', #5840 ) ;
#1228 = LINE ( 'NONE', #7862, #1419 ) ;
#1229 = CARTESIAN_POINT ( 'NONE',  ( 0.5000000000000000000, 10.00000000000000355, -5.999999999999998224 ) ) ;
#1230 = CARTESIAN_POINT ( 'NONE',  ( -10.19839929293505776, 4.531249999044084653, -24.62111388750000174 ) ) ;
#1231 = LINE ( 'NONE', #7145, #1714 ) ;
#1232 = VERTEX_POINT ( 'NONE', #9251 ) ;
#1233 = ORIENTED_EDGE ( 'NONE', *, *, #8133, .T. ) ;
#1234 = CARTESIAN_POINT ( 'NONE',  ( -0.1920286436967143240, 0.000000000000000000, 0.000000000000000000 ) ) ;
#1235 = CARTESIAN_POINT ( 'NONE',  ( -17.40975659021753330, 3.843749999044085097, 17.40975659021752975 ) ) ;
#1236 = CARTESIAN_POINT ( 'NONE',  ( -17.40975659021752975, 4.768749999044085364, -17.40975659021752975 ) ) ;
#1237 = CARTESIAN_POINT ( 'NONE',  ( -4.592425496802574367E-15, 3.750000000000000000, 25.00000000000000000 ) ) ;
#1238 = CARTESIAN_POINT ( 'NONE',  ( 0.000000000000000000, 82.00000000000000000, 0.000000000000000000 ) ) ;
#1239 = DIRECTION ( 'NONE',  ( -1.000000000000000000, 0.000000000000000000, -1.047444401652940007E-14 ) ) ;
#1240 = LINE ( 'NONE', #4680, #1791 ) ;
#1241 = CARTESIAN_POINT ( 'NONE',  ( 5.665063509461120361, 10.00000000000000355, -10.81217782649108372 ) ) ;
#1242 = VECTOR ( 'NONE', #4786, 999.9999999999998863 ) ;
#1243 = TOROIDAL_SURFACE ( 'NONE', #1944, 24.91176187412963117, 3.000000000000000000 ) ;
#1244 = EDGE_LOOP ( 'NONE', ( #5826, #1663, #6426, #7459 ) ) ;
#1245 = ORIENTED_EDGE ( 'NONE', *, *, #699, .T. ) ;
#1246 = PRODUCT_DEFINITION_SHAPE ( 'NONE', 'NONE',  #10949 ) ;
#1247 = VERTEX_POINT ( 'NONE', #7603 ) ;
#1248 = CARTESIAN_POINT ( 'NONE',  ( -3.208128317448977196, 19.34316356887881128, 6.223805082245715603 ) ) ;
#1249 = CIRCLE ( 'NONE', #1405, 5.000000000000000888 ) ;
#1250 = DIRECTION ( 'NONE',  ( 0.000000000000000000, 1.000000000000000000, 0.000000000000000000 ) ) ;
#1251 = DIRECTION ( 'NONE',  ( -0.000000000000000000, -0.000000000000000000, 1.000000000000000000 ) ) ;
#1252 = LINE ( 'NONE', #1354, #7425 ) ;
#1253 = EDGE_CURVE ( 'NONE', #6230, #9320, #6686, .T. ) ;
#1254 = DIRECTION ( 'NONE',  ( 0.8660254037844380415, 0.000000000000000000, 0.5000000000000009992 ) ) ;
#1255 = LINE ( 'NONE', #2784, #3930 ) ;
#1256 = VECTOR ( 'NONE', #5128, 1000.000000000000000 ) ;
#1257 = VECTOR ( 'NONE', #4808, 1000.000000000000000 ) ;
#1258 = ORIENTED_EDGE ( 'NONE', *, *, #525, .F. ) ;
#1259 = ADVANCED_FACE ( 'NONE', ( #5878 ), #9404, .F. ) ;
#1260 = ORIENTED_EDGE ( 'NONE', *, *, #10753, .T. ) ;
#1261 = AXIS2_PLACEMENT_3D ( 'NONE', #3295, #5864, #9221 ) ;
#1262 = FACE_OUTER_BOUND ( 'NONE', #7179, .T. ) ;
#1263 = PLANE ( 'NONE',  #5478 ) ;
#1264 = DIRECTION ( 'NONE',  ( 0.4999999999999949485, 0.000000000000000000, 0.8660254037844415942 ) ) ;
#1265 = CIRCLE ( 'NONE', #212, 2.999999999999999112 ) ;
#1266 = DIRECTION ( 'NONE',  ( 0.2500000000000009992, -0.8660254037844380415, -0.4330127018922199644 ) ) ;
#1267 = ADVANCED_FACE ( 'NONE', ( #9340 ), #5228, .F. ) ;
#1268 = CARTESIAN_POINT ( 'NONE',  ( 28.89716436598705585, 102.6833647615033840, 5.000000000000000000 ) ) ;
#1269 = SHAPE_REPRESENTATION ( 'BR-816', ( #5113, #9855, #5639, #9692, #7765, #8444, #869, #8102, #3872 ), #8096 ) ;
#1270 = EDGE_CURVE ( 'NONE', #10548, #4873, #7811, .T. ) ;
#1271 = EDGE_LOOP ( 'NONE', ( #4840, #1939, #3452, #622, #4084, #2284, #2605, #5069, #10916, #10769, #1975, #6829 ) ) ;
#1272 = CIRCLE ( 'NONE', #4980, 5.000000000000000000 ) ;
#1273 = CARTESIAN_POINT ( 'NONE',  ( 0.000000000000000000, -58.00000000000000000, 27.91176187412963117 ) ) ;
#1274 = DIRECTION ( 'NONE',  ( 0.000000000000000000, -0.4999999999999999445, -0.8660254037844387076 ) ) ;
#1275 = CARTESIAN_POINT ( 'NONE',  ( -19.39162934935757931, 5.000000000000000888, 15.17115553405142947 ) ) ;
#1276 = CARTESIAN_POINT ( 'NONE',  ( 10.19839929293506486, 5.206249999044084475, 24.62111388749999819 ) ) ;
#1277 = ORIENTED_EDGE ( 'NONE', *, *, #2943, .F. ) ;
#1278 = AXIS2_PLACEMENT_3D ( 'NONE', #6452, #2234, #9803 ) ;
#1279 = CARTESIAN_POINT ( 'NONE',  ( -12.77350269189627241, 10.00000000000000355, -1.327078395747997636E-13 ) ) ;
#1280 =( NAMED_UNIT ( * ) SI_UNIT ( $, .STERADIAN. ) SOLID_ANGLE_UNIT ( ) );
#1281 = DIRECTION ( 'NONE',  ( 0.000000000000000000, 0.000000000000000000, 1.000000000000000000 ) ) ;
#1282 = CARTESIAN_POINT ( 'NONE',  ( 17.40975659021752620, 3.093749999044084653, 17.40975659021753330 ) ) ;
#1283 = VECTOR ( 'NONE', #3007, 1000.000000000000000 ) ;
#1284 = ORIENTED_EDGE ( 'NONE', *, *, #6471, .T. ) ;
#1285 = ORIENTED_EDGE ( 'NONE', *, *, #1522, .F. ) ;
#1286 = ORIENTED_EDGE ( 'NONE', *, *, #997, .F. ) ;
#1287 = EDGE_CURVE ( 'NONE', #3078, #448, #6936, .T. ) ;
#1288 = EDGE_LOOP ( 'NONE', ( #4925, #3557, #374, #9513 ) ) ;
#1289 = AXIS2_PLACEMENT_3D ( 'NONE', #7063, #7010, #10421 ) ;
#1290 = DIRECTION ( 'NONE',  ( -1.000000000000000000, -0.000000000000000000, -0.000000000000000000 ) ) ;
#1291 = CARTESIAN_POINT ( 'NONE',  ( 17.40975659021752620, 3.093749999044084653, 17.40975659021753330 ) ) ;
#1292 = CARTESIAN_POINT ( 'NONE',  ( -10.19839929293507552, 4.081249999044084475, 24.62111388749999463 ) ) ;
#1293 = ORIENTED_EDGE ( 'NONE', *, *, #10193, .F. ) ;
#1294 = CARTESIAN_POINT ( 'NONE',  ( 15.13990010960488952, 25.00000000000000000, -5.276923788646758595 ) ) ;
#1295 = DIRECTION ( 'NONE',  ( 0.000000000000000000, -1.000000000000000000, 0.000000000000000000 ) ) ;
#1296 = CIRCLE ( 'NONE', #10816, 4.999999999999987566 ) ;
#1297 = CARTESIAN_POINT ( 'NONE',  ( -10.35533905932737575, 0.9249999980881692396, -25.00000000000000000 ) ) ;
#1298 = PLANE ( 'NONE',  #6558 ) ;
#1299 = ADVANCED_FACE ( 'NONE', ( #3543 ), #3366, .F. ) ;
#1300 = ORIENTED_EDGE ( 'NONE', *, *, #1442, .F. ) ;
#1301 = AXIS2_PLACEMENT_3D ( 'NONE', #9916, #4746, #7268 ) ;
#1302 = DIRECTION ( 'NONE',  ( 0.000000000000000000, 0.000000000000000000, 1.000000000000000000 ) ) ;
#1303 = CIRCLE ( 'NONE', #4668, 2.999999999999997335 ) ;
#1304 = FACE_OUTER_BOUND ( 'NONE', #10765, .T. ) ;
#1305 = VECTOR ( 'NONE', #8382, 1000.000000000000000 ) ;
#1306 = CARTESIAN_POINT ( 'NONE',  ( -17.67766952966369232, 4.237499998088169129, 17.67766952966368876 ) ) ;
#1307 = DIRECTION ( 'NONE',  ( -0.000000000000000000, 1.000000000000000000, -0.000000000000000000 ) ) ;
#1308 = CARTESIAN_POINT ( 'NONE',  ( 1.285879139104720831E-15, 31.00000000000000000, 10.50000000000000000 ) ) ;
#1309 = CARTESIAN_POINT ( 'NONE',  ( -7.276923788646840308, -0.001000000000001000089, -18.60400172474260216 ) ) ;
#1310 = DIRECTION ( 'NONE',  ( 2.168404344971010594E-16, 0.000000000000000000, 1.000000000000000000 ) ) ;
#1311 = CIRCLE ( 'NONE', #412, 10.50000000000000000 ) ;
#1312 = ORIENTED_EDGE ( 'NONE', *, *, #7953, .F. ) ;
#1313 = CARTESIAN_POINT ( 'NONE',  ( 0.000000000000000000, 85.00000000000000000, 0.000000000000000000 ) ) ;
#1314 = DIRECTION ( 'NONE',  ( 0.000000000000000000, 0.000000000000000000, -1.000000000000000000 ) ) ;
#1315 = LINE ( 'NONE', #7318, #7623 ) ;
#1316 = FACE_OUTER_BOUND ( 'NONE', #4208, .T. ) ;
#1317 = CARTESIAN_POINT ( 'NONE',  ( -19.75000000000003197, 25.00000000000000000, -2.999999999999789946 ) ) ;
#1318 = ORIENTED_EDGE ( 'NONE', *, *, #1514, .F. ) ;
#1319 = VERTEX_POINT ( 'NONE', #6766 ) ;
#1320 = EDGE_CURVE ( 'NONE', #10806, #10642, #2710, .T. ) ;
#1321 = EDGE_CURVE ( 'NONE', #3052, #6508, #10023, .T. ) ;
#1322 = EDGE_CURVE ( 'NONE', #6596, #4397, #183, .T. ) ;
#1323 = CARTESIAN_POINT ( 'NONE',  ( 0.000000000000000000, -55.00000000000000000, -24.91176187412963117 ) ) ;
#1324 = CARTESIAN_POINT ( 'NONE',  ( 12.47307621135322186, 28.00000000000000000, -15.60400172474273717 ) ) ;
#1325 = CARTESIAN_POINT ( 'NONE',  ( 17.40975659021752975, 4.518749999044084475, -17.40975659021752975 ) ) ;
#1326 = ORIENTED_EDGE ( 'NONE', *, *, #10181, .F. ) ;
#1327 = CARTESIAN_POINT ( 'NONE',  ( -6.296693311223937606, 10.00000000000000355, 3.058047309049956475 ) ) ;
#1328 = CARTESIAN_POINT ( 'NONE',  ( 1.530808498934191521E-15, 2.862499998088169573, -25.00000000000000000 ) ) ;
#1329 = CARTESIAN_POINT ( 'NONE',  ( 24.62111388750000174, 1.218749999044084431, 0.000000000000000000 ) ) ;
#1330 = CARTESIAN_POINT ( 'NONE',  ( 17.67766952966369232, 0.1249999999999999722, -17.67766952966369232 ) ) ;
#1331 = EDGE_CURVE ( 'NONE', #716, #8104, #5972, .T. ) ;
#1332 = PRODUCT ( 'lid', 'lid', '', ( #9152 ) ) ;
#1333 = ORIENTED_EDGE ( 'NONE', *, *, #2241, .T. ) ;
#1334 = VERTEX_POINT ( 'NONE', #1020 ) ;
#1335 = ORIENTED_EDGE ( 'NONE', *, *, #5586, .T. ) ;
#1336 = EDGE_CURVE ( 'NONE', #6439, #3577, #843, .T. ) ;
#1337 = CARTESIAN_POINT ( 'NONE',  ( -2.999999999999999112, 28.00000000000000000, -19.75000000000000000 ) ) ;
#1338 = CARTESIAN_POINT ( 'NONE',  ( -17.40975659021752975, 4.593749999044084653, -17.40975659021752975 ) ) ;
#1339 = CARTESIAN_POINT ( 'NONE',  ( 24.62111388750000174, 3.456249999044084920, -10.19839929293505776 ) ) ;
#1340 = CARTESIAN_POINT ( 'NONE',  ( 10.35533905932738286, 2.812500000000000000, 24.99999999999999645 ) ) ;
#1341 = CARTESIAN_POINT ( 'NONE',  ( 0.000000000000000000, 1.000000000000001998, 0.5773502691896277295 ) ) ;
#1342 = CARTESIAN_POINT ( 'NONE',  ( -25.00000000000000000, 2.049999998088169129, -10.35533905932738108 ) ) ;
#1343 = CARTESIAN_POINT ( 'NONE',  ( 0.000000000000000000, 25.00000000000000000, 0.000000000000000000 ) ) ;
#1344 = CARTESIAN_POINT ( 'NONE',  ( 10.35533905932738286, 3.424999998088169129, 24.99999999999999645 ) ) ;
#1345 = EDGE_CURVE ( 'NONE', #8432, #10429, #10558, .T. ) ;
#1346 = ORIENTED_EDGE ( 'NONE', *, *, #6014, .T. ) ;
#1347 = ORIENTED_EDGE ( 'NONE', *, *, #414, .T. ) ;
#1348 = ORIENTED_EDGE ( 'NONE', *, *, #1803, .T. ) ;
#1349 = CARTESIAN_POINT ( 'NONE',  ( -17.67766952966368876, 0.3750000000000000000, -17.67766952966369232 ) ) ;
#1350 = CARTESIAN_POINT ( 'NONE',  ( -10.35533905932735621, 4.687500000000000888, 25.00000000000003197 ) ) ;
#1351 = CARTESIAN_POINT ( 'NONE',  ( 82.32050807568876394, 100.2820323027551268, -3.379762621896238883 ) ) ;
#1352 = LINE ( 'NONE', #2121, #5707 ) ;
#1353 = CARTESIAN_POINT ( 'NONE',  ( -9.874999999999777955, 28.00000000000000000, 20.10400172474279401 ) ) ;
#1354 = CARTESIAN_POINT ( 'NONE',  ( 24.81055694375000087, 0.5031249985661269131, 0.000000000000000000 ) ) ;
#1355 = CARTESIAN_POINT ( 'NONE',  ( 17.40975659021752975, 0.3437499990440845421, -17.40975659021752975 ) ) ;
#1356 = DIRECTION ( 'NONE',  ( 0.000000000000000000, 0.000000000000000000, -1.000000000000000000 ) ) ;
#1357 = ORIENTED_EDGE ( 'NONE', *, *, #1253, .T. ) ;
#1358 = ORIENTED_EDGE ( 'NONE', *, *, #9661, .T. ) ;
#1359 = ORIENTED_EDGE ( 'NONE', *, *, #2795, .T. ) ;
#1360 = STYLED_ITEM ( 'NONE', ( #2425 ), #9406 ) ;
#1361 = CARTESIAN_POINT ( 'NONE',  ( 0.000000000000000000, 0.000000000000000000, -25.00000000000000000 ) ) ;
#1362 = CARTESIAN_POINT ( 'NONE',  ( 0.000000000000000000, 20.00000000000000355, 0.000000000000000000 ) ) ;
#1363 = CARTESIAN_POINT ( 'NONE',  ( -4.592425496802574367E-15, 3.750000000000000000, 25.00000000000000000 ) ) ;
#1364 = DIRECTION ( 'NONE',  ( 0.000000000000000000, 0.000000000000000000, 1.000000000000000000 ) ) ;
#1365 = VECTOR ( 'NONE', #5254, 1000.000000000000000 ) ;
#1366 = ORIENTED_EDGE ( 'NONE', *, *, #3618, .F. ) ;
#1367 = VERTEX_POINT ( 'NONE', #1726 ) ;
#1368 = CARTESIAN_POINT ( 'NONE',  ( -3.716506350946151116, 19.75000000000000000, 5.437177826491034871 ) ) ;
#1369 = CARTESIAN_POINT ( 'NONE',  ( -19.05903902044739695, 4.999999999999999112, -16.17878337876688022 ) ) ;
#1370 = CARTESIAN_POINT ( 'NONE',  ( -10.19839929293507375, 5.081249999044084475, 24.62111388749999108 ) ) ;
#1371 = ORIENTED_EDGE ( 'NONE', *, *, #2509, .F. ) ;
#1372 = DIRECTION ( 'NONE',  ( 0.000000000000000000, 1.000000000000000000, 0.000000000000000000 ) ) ;
#1373 = CARTESIAN_POINT ( 'NONE',  ( -0.5000000000000000000, 19.03096903053429756, 6.982120021884467675 ) ) ;
#1374 = CIRCLE ( 'NONE', #1916, 20.00000000000000000 ) ;
#1375 = CARTESIAN_POINT ( 'NONE',  ( 10.19839929293505953, 2.406249999044085541, -24.62111388750000174 ) ) ;
#1376 = CARTESIAN_POINT ( 'NONE',  ( 17.67766952966369232, 2.737499998088169573, -17.67766952966369232 ) ) ;
#1377 = ADVANCED_FACE ( 'NONE', ( #8628 ), #5102, .F. ) ;
#1378 = EDGE_LOOP ( 'NONE', ( #10791, #2872, #5728 ) ) ;
#1379 = AXIS2_PLACEMENT_3D ( 'NONE', #4184, #10264, #5902 ) ;
#1380 = EDGE_CURVE ( 'NONE', #20, #748, #2431, .T. ) ;
#1381 = CARTESIAN_POINT ( 'NONE',  ( -24.62111388750000174, 0.8312499990440843645, -10.19839929293506131 ) ) ;
#1382 = DIRECTION ( 'NONE',  ( 0.000000000000000000, 1.000000000000000000, 0.000000000000000000 ) ) ;
#1383 = CARTESIAN_POINT ( 'NONE',  ( -24.62111388750000174, 3.831249999044084920, -10.19839929293506131 ) ) ;
#1384 = CARTESIAN_POINT ( 'NONE',  ( -17.67766952966369232, 4.625000000000000000, 17.67766952966368876 ) ) ;
#1385 =( BOUNDED_CURVE ( )  B_SPLINE_CURVE ( 2, ( #7665, #9200, #3274, #156, #10089 ),
 .UNSPECIFIED., .F., .F. ) 
 B_SPLINE_CURVE_WITH_KNOTS ( ( 3, 2, 3 ),
 ( 0.9500000000000000666, 0.9750000000000000888, 1.000000000000000000 ),
 .UNSPECIFIED. ) 
 CURVE ( )  GEOMETRIC_REPRESENTATION_ITEM ( )  RATIONAL_B_SPLINE_CURVE ( ( 0.9999999999999996669, 0.9238795325112870716, 1.000000000000000000, 0.9238795325112867385, 1.000000000000000000 ) ) 
 REPRESENTATION_ITEM ( '' )  );
#1386 = FACE_OUTER_BOUND ( 'NONE', #3015, .T. ) ;
#1387 = DIRECTION ( 'NONE',  ( 0.000000000000000000, 1.000000000000000000, 0.000000000000000000 ) ) ;
#1388 = DIRECTION ( 'NONE',  ( 0.000000000000000000, 0.000000000000000000, 1.000000000000000000 ) ) ;
#1389 = LINE ( 'NONE', #1502, #10598 ) ;
#1390 = EDGE_CURVE ( 'NONE', #9703, #8735, #3858, .T. ) ;
#1391 = ORIENTED_EDGE ( 'NONE', *, *, #1336, .F. ) ;
#1392 = EDGE_LOOP ( 'NONE', ( #5015, #7159, #4615, #6449 ) ) ;
#1393 = ORIENTED_EDGE ( 'NONE', *, *, #3624, .T. ) ;
#1394 = VERTEX_POINT ( 'NONE', #10347 ) ;
#1395 = UNCERTAINTY_MEASURE_WITH_UNIT (LENGTH_MEASURE( 1.000000000000000082E-05 ), #2530, 'distance_accuracy_value', 'NONE');
#1396 = LINE ( 'NONE', #4580, #3474 ) ;
#1397 = ADVANCED_FACE ( 'NONE', ( #3603 ), #1785, .F. ) ;
#1398 = DIRECTION ( 'NONE',  ( 1.000000000000000000, 0.000000000000000000, 0.000000000000000000 ) ) ;
#1399 = CARTESIAN_POINT ( 'NONE',  ( 17.67766952966369232, 1.737499998088169351, -17.67766952966369232 ) ) ;
#1400 = AXIS2_PLACEMENT_3D ( 'NONE', #7820, #2766, #461 ) ;
#1401 = FACE_OUTER_BOUND ( 'NONE', #2174, .T. ) ;
#1402 = CYLINDRICAL_SURFACE ( 'NONE', #8139, 6.999999999999997335 ) ;
#1403 = DIRECTION ( 'NONE',  ( 0.000000000000000000, 0.000000000000000000, 1.000000000000000000 ) ) ;
#1404 = DIRECTION ( 'NONE',  ( -0.000000000000000000, 1.000000000000000000, -0.000000000000000000 ) ) ;
#1405 = AXIS2_PLACEMENT_3D ( 'NONE', #5689, #9982, #9871 ) ;
#1406 = AXIS2_PLACEMENT_3D ( 'NONE', #1323, #7180, #10444 ) ;
#1407 = EDGE_CURVE ( 'NONE', #4897, #9663, #7369, .T. ) ;
#1408 = ORIENTED_EDGE ( 'NONE', *, *, #7379, .F. ) ;
#1409 = ORIENTED_EDGE ( 'NONE', *, *, #10098, .F. ) ;
#1410 = LINE ( 'NONE', #10588, #10799 ) ;
#1411 = DIRECTION ( 'NONE',  ( -0.000000000000000000, 1.000000000000000000, -0.000000000000000000 ) ) ;
#1412 = CARTESIAN_POINT ( 'NONE',  ( 10.35533905932734733, 4.799999998088170905, -25.00000000000004263 ) ) ;
#1413 = AXIS2_PLACEMENT_3D ( 'NONE', #2827, #6168, #5342 ) ;
#1414 = AXIS2_PLACEMENT_3D ( 'NONE', #7498, #1757, #3275 ) ;
#1415 = CARTESIAN_POINT ( 'NONE',  ( -4.592425496802574367E-15, 0.7500000000000000000, 25.00000000000000000 ) ) ;
#1416 = CARTESIAN_POINT ( 'NONE',  ( 2.999999999999997335, -0.001000000000001000089, -15.75000000000000355 ) ) ;
#1417 = ORIENTED_EDGE ( 'NONE', *, *, #2410, .T. ) ;
#1418 = AXIS2_PLACEMENT_3D ( 'NONE', #6999, #2218, #3946 ) ;
#1419 = VECTOR ( 'NONE', #2096, 1000.000000000000000 ) ;
#1420 =( NAMED_UNIT ( * ) SI_UNIT ( $, .STERADIAN. ) SOLID_ANGLE_UNIT ( ) );
#1421 = CARTESIAN_POINT ( 'NONE',  ( -24.62111388750000174, 2.893749999044084475, -3.015216831376932151E-15 ) ) ;
#1422 = VERTEX_POINT ( 'NONE', #1337 ) ;
#1423 = CARTESIAN_POINT ( 'NONE',  ( 24.99999999999999289, 2.549999998088169129, 10.35533905932739529 ) ) ;
#1424 = VERTEX_POINT ( 'NONE', #2760 ) ;
#1425 = CARTESIAN_POINT ( 'NONE',  ( -9.474358296526972367, 10.00000000000000355, 2.857142857142765724 ) ) ;
#1426 = CARTESIAN_POINT ( 'NONE',  ( 1.507608415688466075E-15, 3.468749999044085097, -24.62111388750000174 ) ) ;
#1427 = VERTEX_POINT ( 'NONE', #4516 ) ;
#1428 = ORIENTED_EDGE ( 'NONE', *, *, #8893, .T. ) ;
#1429 = VERTEX_POINT ( 'NONE', #2875 ) ;
#1430 = CARTESIAN_POINT ( 'NONE',  ( 1.530808498934191521E-15, 4.862499998088169129, -25.00000000000000000 ) ) ;
#1431 = DIRECTION ( 'NONE',  ( 0.000000000000000000, 1.000000000000000000, 0.000000000000000000 ) ) ;
#1432 = CARTESIAN_POINT ( 'NONE',  ( 24.62111388750000174, 3.218749999044084653, 0.000000000000000000 ) ) ;
#1433 = VERTEX_POINT ( 'NONE', #4565 ) ;
#1434 = EDGE_CURVE ( 'NONE', #7845, #10020, #3873, .T. ) ;
#1435 = PLANE ( 'NONE',  #3146 ) ;
#1436 = CIRCLE ( 'NONE', #6396, 2.999999999999999112 ) ;
#1437 = CARTESIAN_POINT ( 'NONE',  ( -17.67766952966368876, 1.987499998088169129, -17.67766952966369232 ) ) ;
#1438 = CARTESIAN_POINT ( 'NONE',  ( 10.35533905932738286, 1.424999998088169129, 24.99999999999999645 ) ) ;
#1439 = LINE ( 'NONE', #2167, #7262 ) ;
#1440 = CARTESIAN_POINT ( 'NONE',  ( 10.35533905932737930, 3.799999998088170461, -25.00000000000000000 ) ) ;
#1441 = AXIS2_PLACEMENT_3D ( 'NONE', #9150, #10878, #939 ) ;
#1442 = EDGE_CURVE ( 'NONE', #10157, #7784, #7920, .T. ) ;
#1443 = ORIENTED_EDGE ( 'NONE', *, *, #6772, .F. ) ;
#1444 = ORIENTED_EDGE ( 'NONE', *, *, #5501, .F. ) ;
#1445 = ORIENTED_EDGE ( 'NONE', *, *, #3645, .T. ) ;
#1446 = VERTEX_POINT ( 'NONE', #8690 ) ;
#1447 = CIRCLE ( 'NONE', #4129, 12.77350269189627063 ) ;
#1448 = AXIS2_PLACEMENT_3D ( 'NONE', #4540, #3796, #1356 ) ;
#1449 = ORIENTED_EDGE ( 'NONE', *, *, #5130, .T. ) ;
#1450 = ADVANCED_FACE ( 'NONE', ( #6159 ), #10559, .F. ) ;
#1451 =( BOUNDED_CURVE ( )  B_SPLINE_CURVE ( 3, ( #1206, #3737, #2076, #3901 ),
 .UNSPECIFIED., .F., .F. ) 
 B_SPLINE_CURVE_WITH_KNOTS ( ( 4, 4 ),
 ( 3.927175151554405552, 3.998664601439926081 ),
 .UNSPECIFIED. ) 
 CURVE ( )  GEOMETRIC_REPRESENTATION_ITEM ( )  RATIONAL_B_SPLINE_CURVE ( ( 1.000000000000000000, 0.9995741502243209453, 0.9995741502243209453, 1.000000000000000000 ) ) 
 REPRESENTATION_ITEM ( '' )  );
#1452 = EDGE_CURVE ( 'NONE', #10359, #9337, #5390, .T. ) ;
#1453 = CIRCLE ( 'NONE', #2154, 6.975000000000008527 ) ;
#1454 = CARTESIAN_POINT ( 'NONE',  ( 3.061616997868383043E-15, 0.000000000000000000, 25.00000000000000000 ) ) ;
#1455 = EDGE_CURVE ( 'NONE', #7330, #4112, #10426, .T. ) ;
#1456 = LINE ( 'NONE', #324, #9119 ) ;
#1457 = AXIS2_PLACEMENT_3D ( 'NONE', #1881, #4430, #2626 ) ;
#1458 = EDGE_LOOP ( 'NONE', ( #10032, #6332, #5618, #10903 ) ) ;
#1459 = DIRECTION ( 'NONE',  ( -1.000000000000000000, 0.000000000000000000, 0.000000000000000000 ) ) ;
#1460 = DIRECTION ( 'NONE',  ( -0.8660254037844345998, 0.000000000000000000, -0.5000000000000071054 ) ) ;
#1461 = CIRCLE ( 'NONE', #3767, 2.999999999999999112 ) ;
#1462 = CARTESIAN_POINT ( 'NONE',  ( -10.19839929293505776, 0.5312499990440845421, -24.62111388750000174 ) ) ;
#1463 = CARTESIAN_POINT ( 'NONE',  ( -25.00000000000001066, 3.562500000000000000, 10.35533905932737397 ) ) ;
#1464 = EDGE_CURVE ( 'NONE', #824, #4079, #8657, .T. ) ;
#1465 = CIRCLE ( 'NONE', #6577, 30.00000000000000000 ) ;
#1466 = EDGE_LOOP ( 'NONE', ( #9188, #419, #9134, #2277, #8530 ) ) ;
#1467 = ORIENTED_EDGE ( 'NONE', *, *, #6471, .F. ) ;
#1468 = AXIS2_PLACEMENT_3D ( 'NONE', #5195, #2673, #1693 ) ;
#1469 = ORIENTED_EDGE ( 'NONE', *, *, #10521, .T. ) ;
#1470 = VECTOR ( 'NONE', #9381, 1000.000000000000000 ) ;
#1471 = EDGE_CURVE ( 'NONE', #3766, #806, #8902, .T. ) ;
#1472 = PLANE ( 'NONE',  #4474 ) ;
#1473 = VECTOR ( 'NONE', #5246, 1000.000000000000000 ) ;
#1474 = DIRECTION ( 'NONE',  ( 0.000000000000000000, -1.000000000000000000, 0.000000000000000000 ) ) ;
#1475 = CARTESIAN_POINT ( 'NONE',  ( 0.000000000000000000, 10.10000000000000497, 0.000000000000000000 ) ) ;
#1476 = CARTESIAN_POINT ( 'NONE',  ( -12.13990010960478827, 28.00000000000000000, 10.47307621135345990 ) ) ;
#1477 = CARTESIAN_POINT ( 'NONE',  ( 1.500000000000001332, 7.400000000000008349, 2.168404344971008868E-16 ) ) ;
#1478 = EDGE_CURVE ( 'NONE', #4041, #7282, #3720, .T. ) ;
#1479 = CIRCLE ( 'NONE', #8350, 2.999999999999996891 ) ;
#1480 = ORIENTED_EDGE ( 'NONE', *, *, #7319, .F. ) ;
#1481 = CARTESIAN_POINT ( 'NONE',  ( 12.47307621135322186, -0.001000000000001000089, -15.60400172474273717 ) ) ;
#1482 = CYLINDRICAL_SURFACE ( 'NONE', #9492, 6.975000000000008527 ) ;
#1483 = CARTESIAN_POINT ( 'NONE',  ( -10.19839929293507375, 2.081249999044084920, 24.62111388749999108 ) ) ;
#1484 = ORIENTED_EDGE ( 'NONE', *, *, #3967, .F. ) ;
#1485 = CYLINDRICAL_SURFACE ( 'NONE', #4776, 2.999999999999997780 ) ;
#1486 = APPLICATION_PROTOCOL_DEFINITION ( 'draft international standard', 'automotive_design', 1998, #9136 ) ;
#1487 = PLANE ( 'NONE',  #3213 ) ;
#1488 = ORIENTED_EDGE ( 'NONE', *, *, #7002, .F. ) ;
#1489 = CARTESIAN_POINT ( 'NONE',  ( 18.60400172474263414, 28.00000000000000000, -7.276923788646775471 ) ) ;
#1490 = CARTESIAN_POINT ( 'NONE',  ( 24.62111388750000174, 0.2187499990440845699, 0.000000000000000000 ) ) ;
#1491 = ORIENTED_EDGE ( 'NONE', *, *, #636, .T. ) ;
#1492 = ORIENTED_EDGE ( 'NONE', *, *, #2347, .T. ) ;
#1493 = ORIENTED_EDGE ( 'NONE', *, *, #9010, .T. ) ;
#1494 = CARTESIAN_POINT ( 'NONE',  ( -25.00000000000000000, 3.049999998088169129, -10.35533905932738108 ) ) ;
#1495 = CARTESIAN_POINT ( 'NONE',  ( 24.62111388750000174, 5.218749999044084653, 0.000000000000000000 ) ) ;
#1496 = CARTESIAN_POINT ( 'NONE',  ( -17.40975659021753330, 3.843749999044085097, 17.40975659021752975 ) ) ;
#1497 = EDGE_LOOP ( 'NONE', ( #5465, #8707, #5889, #9627 ) ) ;
#1498 = FACE_BOUND ( 'NONE', #8807, .T. ) ;
#1499 = SHAPE_REPRESENTATION_RELATIONSHIP ( 'NONE' , 'NONE' ,  #2382, #9406 ) ;
#1500 = DIRECTION ( 'NONE',  ( -0.000000000000000000, -1.000000000000000000, -0.000000000000000000 ) ) ;
#1501 = LINE ( 'NONE', #1717, #5855 ) ;
#1502 = CARTESIAN_POINT ( 'NONE',  ( -10.00000000000000000, 93.00000000000001421, -5.000000000000000000 ) ) ;
#1503 = ORIENTED_EDGE ( 'NONE', *, *, #6130, .T. ) ;
#1504 = UNCERTAINTY_MEASURE_WITH_UNIT (LENGTH_MEASURE( 1.000000000000000082E-05 ), #9671, 'distance_accuracy_value', 'NONE');
#1505 = CARTESIAN_POINT ( 'NONE',  ( 82.32050807568876394, 89.28203230275514102, 0.000000000000000000 ) ) ;
#1506 = DIRECTION ( 'NONE',  ( 0.000000000000000000, 0.000000000000000000, 1.000000000000000000 ) ) ;
#1507 = CARTESIAN_POINT ( 'NONE',  ( 0.3808229674253814645, 5.000000000000004441, 24.72275166764144316 ) ) ;
#1508 = CARTESIAN_POINT ( 'NONE',  ( -1.214306433183764808E-14, 10.00000000000000355, -12.77350269189627063 ) ) ;
#1509 = CARTESIAN_POINT ( 'NONE',  ( 10.19839929293505953, 0.4062499990440845421, -24.62111388750000174 ) ) ;
#1510 = DIRECTION ( 'NONE',  ( -0.000000000000000000, 1.000000000000000000, -0.000000000000000000 ) ) ;
#1511 = EDGE_LOOP ( 'NONE', ( #9359, #9062, #8305, #4763 ) ) ;
#1512 = EDGE_CURVE ( 'NONE', #7692, #795, #8292, .T. ) ;
#1513 = VERTEX_POINT ( 'NONE', #7872 ) ;
#1514 = EDGE_CURVE ( 'NONE', #4593, #7190, #7098, .T. ) ;
#1515 = VERTEX_POINT ( 'NONE', #9629 ) ;
#1516 = EDGE_CURVE ( 'NONE', #399, #8258, #4076, .T. ) ;
#1517 = DIRECTION ( 'NONE',  ( 0.000000000000000000, -1.000000000000000000, 0.000000000000000000 ) ) ;
#1518 = CARTESIAN_POINT ( 'NONE',  ( -20.63749999999999574, 1.047786282324291578E-15, 6.975000000000008527 ) ) ;
#1519 = CARTESIAN_POINT ( 'NONE',  ( 11.16025403784440329, 90.66987298107783033, -5.000000000000000000 ) ) ;
#1520 = CARTESIAN_POINT ( 'NONE',  ( 10.35533905932737930, 1.187500000000000000, -25.00000000000000000 ) ) ;
#1521 = DIRECTION ( 'NONE',  ( 0.000000000000000000, -0.000000000000000000, 1.000000000000000000 ) ) ;
#1522 = EDGE_CURVE ( 'NONE', #10165, #9038, #6375, .T. ) ;
#1523 = ORIENTED_EDGE ( 'NONE', *, *, #3552, .T. ) ;
#1524 = ORIENTED_EDGE ( 'NONE', *, *, #3129, .T. ) ;
#1525 = EDGE_CURVE ( 'NONE', #2067, #3638, #5542, .T. ) ;
#1526 = SURFACE_SIDE_STYLE ('',( #9925 ) ) ;
#1527 = PRESENTATION_STYLE_ASSIGNMENT (( #4081 ) ) ;
#1528 = CARTESIAN_POINT ( 'NONE',  ( 10.19839929293505953, 0.5812499990440844755, -24.62111388750000174 ) ) ;
#1529 = ORIENTED_EDGE ( 'NONE', *, *, #414, .F. ) ;
#1530 = CARTESIAN_POINT ( 'NONE',  ( 10.35640646055103886, 93.66987298107783033, 5.000000000000000000 ) ) ;
#1531 = APPLICATION_PROTOCOL_DEFINITION ( 'draft international standard', 'automotive_design', 1998, #7440 ) ;
#1532 = CARTESIAN_POINT ( 'NONE',  ( -12.47307621135344391, 25.00000000000000000, -15.60400172474256131 ) ) ;
#1533 = ORIENTED_EDGE ( 'NONE', *, *, #1752, .F. ) ;
#1534 = VECTOR ( 'NONE', #4374, 1000.000000000000000 ) ;
#1535 = CARTESIAN_POINT ( 'NONE',  ( -25.00000000000001066, 1.562500000000000000, 10.35533905932737397 ) ) ;
#1536 = CARTESIAN_POINT ( 'NONE',  ( 24.62111388749999108, 1.156249999044084431, 10.19839929293507730 ) ) ;
#1537 = TOROIDAL_SURFACE ( 'NONE', #8419, 5.100000000000000533, 0.1000000000000001582 ) ;
#1538 = ORIENTED_EDGE ( 'NONE', *, *, #4642, .F. ) ;
#1539 = ORIENTED_EDGE ( 'NONE', *, *, #1741, .T. ) ;
#1540 = COLOUR_RGB ( '', 0.09019608, 0.27058824, 0.51372549) ;
#1541 = EDGE_CURVE ( 'NONE', #3501, #5714, #9841, .T. ) ;
#1542 = CARTESIAN_POINT ( 'NONE',  ( 10.35533905932737930, 3.799999998088170017, -25.00000000000000000 ) ) ;
#1543 = CARTESIAN_POINT ( 'NONE',  ( 0.000000000000000000, 0.000000000000000000, 0.000000000000000000 ) ) ;
#1544 = VECTOR ( 'NONE', #2310, 1000.000000000000000 ) ;
#1545 = CARTESIAN_POINT ( 'NONE',  ( 17.40975659021752620, 3.093749999044084653, 17.40975659021753330 ) ) ;
#1546 = EDGE_LOOP ( 'NONE', ( #1782, #8978, #2188, #647 ) ) ;
#1547 = PLANE ( 'NONE',  #1764 ) ;
#1548 = PRESENTATION_STYLE_ASSIGNMENT (( #5045 ) ) ;
#1549 = DIRECTION ( 'NONE',  ( -0.4999999999999947820, 0.000000000000000000, 0.8660254037844417052 ) ) ;
#1550 = DIRECTION ( 'NONE',  ( 0.000000000000000000, 0.000000000000000000, -1.000000000000000000 ) ) ;
#1551 = CARTESIAN_POINT ( 'NONE',  ( -6.305607966083967675, 7.781088913245563177, 11.92163336986826216 ) ) ;
#1552 = CARTESIAN_POINT ( 'NONE',  ( -5.796693311223946488, 10.00000000000000355, 3.924072712834398846 ) ) ;
#1553 = CARTESIAN_POINT ( 'NONE',  ( -13.47724133595217744, 7.781088913245558736, 0.4999999999998588351 ) ) ;
#1554 = COLOUR_RGB ( '', 0.08235294, 0.09019608, 0.10196078) ;
#1555 = AXIS2_PLACEMENT_3D ( 'NONE', #3516, #95, #35 ) ;
#1556 = ORIENTED_EDGE ( 'NONE', *, *, #2418, .T. ) ;
#1557 = ORIENTED_EDGE ( 'NONE', *, *, #2141, .T. ) ;
#1558 = CARTESIAN_POINT ( 'NONE',  ( 10.19839929293506486, 2.031249999044084653, 24.62111388749999819 ) ) ;
#1559 = CARTESIAN_POINT ( 'NONE',  ( -12.13990010960478827, 25.00000000000000000, 10.47307621135345634 ) ) ;
#1560 = ORIENTED_EDGE ( 'NONE', *, *, #2792, .F. ) ;
#1561 = CARTESIAN_POINT ( 'NONE',  ( -10.65103055884460836, 4.999999999999998224, 22.31395431344387603 ) ) ;
#1562 = DIRECTION ( 'NONE',  ( 0.000000000000000000, -1.000000000000000000, 0.000000000000000000 ) ) ;
#1563 = CARTESIAN_POINT ( 'NONE',  ( 0.000000000000000000, 20.00000000000000355, 6.999999999999997335 ) ) ;
#1564 = CARTESIAN_POINT ( 'NONE',  ( -4.522825247065398226E-15, 3.968749999044084209, 24.62111388750000174 ) ) ;
#1565 = CARTESIAN_POINT ( 'NONE',  ( -0.4330127018922190207, 0.000000000000000000, -0.2500000000000004996 ) ) ;
#1566 = ORIENTED_EDGE ( 'NONE', *, *, #5716, .F. ) ;
#1567 = VERTEX_POINT ( 'NONE', #5711 ) ;
#1568 = PRODUCT_DEFINITION_FORMATION_WITH_SPECIFIED_SOURCE ( 'ANY', '', #10587, .NOT_KNOWN. ) ;
#1569 = FACE_OUTER_BOUND ( 'NONE', #3975, .T. ) ;
#1570 = ADVANCED_FACE ( 'NONE', ( #7407 ), #150, .F. ) ;
#1571 = CARTESIAN_POINT ( 'NONE',  ( -6.999999999999998224, 19.66631150450992749, 0.1668442477449725569 ) ) ;
#1572 = CARTESIAN_POINT ( 'NONE',  ( 0.000000000000000000, -8.000000000000000000, 0.000000000000000000 ) ) ;
#1573 = CARTESIAN_POINT ( 'NONE',  ( 25.00000000000000000, 4.062500000000000000, -10.35533905932737753 ) ) ;
#1574 = CARTESIAN_POINT ( 'NONE',  ( 10.29762009200904949, 5.000000000000000000, 22.44659794629365024 ) ) ;
#1575 = VECTOR ( 'NONE', #3300, 1000.000000000000000 ) ;
#1576 = EDGE_CURVE ( 'NONE', #1567, #10596, #8541, .T. ) ;
#1577 = EDGE_LOOP ( 'NONE', ( #2318, #1198, #4126, #7882 ) ) ;
#1578 = CIRCLE ( 'NONE', #7405, 5.750000000000006217 ) ;
#1579 = CARTESIAN_POINT ( 'NONE',  ( 0.000000000000000000, 5.000000000000000000, 0.000000000000000000 ) ) ;
#1580 = LINE ( 'NONE', #9867, #4734 ) ;
#1581 = VECTOR ( 'NONE', #8736, 1000.000000000000000 ) ;
#1582 = DIRECTION ( 'NONE',  ( 0.000000000000000000, 1.000000000000000000, 0.000000000000000000 ) ) ;
#1583 = ORIENTED_EDGE ( 'NONE', *, *, #3129, .F. ) ;
#1584 = EDGE_CURVE ( 'NONE', #9550, #6584, #3570, .T. ) ;
#1585 = CARTESIAN_POINT ( 'NONE',  ( 17.67766952966368521, 3.487499998088169129, 17.67766952966369232 ) ) ;
#1586 = CARTESIAN_POINT ( 'NONE',  ( 0.000000000000000000, 10.10000000000000497, 0.000000000000000000 ) ) ;
#1587 = APPLICATION_CONTEXT ( 'automotive_design' ) ;
#1588 = ADVANCED_FACE ( 'NONE', ( #6010 ), #1161, .F. ) ;
#1589 = LINE ( 'NONE', #4975, #10478 ) ;
#1590 = CARTESIAN_POINT ( 'NONE',  ( 2.999999999999996447, 28.00000000000000000, -19.75000000000000000 ) ) ;
#1591 = CARTESIAN_POINT ( 'NONE',  ( -2.999999999999997335, 28.00000000000000000, 15.75000000000000355 ) ) ;
#1592 = EDGE_CURVE ( 'NONE', #6402, #10131, #6909, .T. ) ;
#1593 = VECTOR ( 'NONE', #9696, 1000.000000000000000 ) ;
#1594 = ORIENTED_EDGE ( 'NONE', *, *, #4781, .F. ) ;
#1595 = MECHANICAL_DESIGN_GEOMETRIC_PRESENTATION_REPRESENTATION (  '', ( #7787 ), #10427 ) ;
#1596 = ORIENTED_EDGE ( 'NONE', *, *, #5849, .T. ) ;
#1597 = CARTESIAN_POINT ( 'NONE',  ( 17.67766952966368521, 5.487499998088169129, 17.67766952966369232 ) ) ;
#1598 = CARTESIAN_POINT ( 'NONE',  ( 7.276923788646575630, 28.00000000000000000, -18.60400172474270519 ) ) ;
#1599 = CARTESIAN_POINT ( 'NONE',  ( 17.40975659021752620, 2.093749999044084653, 17.40975659021753330 ) ) ;
#1600 = CARTESIAN_POINT ( 'NONE',  ( 17.10400172474261637, -0.001000000000001000089, -9.875000000000085265 ) ) ;
#1601 = ORIENTED_EDGE ( 'NONE', *, *, #6187, .F. ) ;
#1602 = DIRECTION ( 'NONE',  ( 0.000000000000000000, -0.8660254037844387076, 0.5000000000000001110 ) ) ;
#1603 = FACE_OUTER_BOUND ( 'NONE', #2945, .T. ) ;
#1604 = CARTESIAN_POINT ( 'NONE',  ( 19.74999999999998934, 28.00000000000000000, -3.000000000000067946 ) ) ;
#1605 = DIRECTION ( 'NONE',  ( -0.2500000000000041078, -0.8660254037844380415, 0.4330127018922182436 ) ) ;
#1606 = CARTESIAN_POINT ( 'NONE',  ( 7.211537444790402596, 10.00000000000000355, 6.776463540776813232 ) ) ;
#1607 = DIRECTION ( 'NONE',  ( 0.000000000000000000, -2.775557561562887961E-17, -1.000000000000000000 ) ) ;
#1608 = CIRCLE ( 'NONE', #19, 28.00000000000000000 ) ;
#1609 = EDGE_CURVE ( 'NONE', #5353, #2588, #2732, .T. ) ;
#1610 = EDGE_CURVE ( 'NONE', #5184, #10316, #1922, .T. ) ;
#1611 = ORIENTED_EDGE ( 'NONE', *, *, #45, .F. ) ;
#1612 = ORIENTED_EDGE ( 'NONE', *, *, #9694, .F. ) ;
#1613 = ORIENTED_EDGE ( 'NONE', *, *, #855, .F. ) ;
#1614 =( BOUNDED_CURVE ( )  B_SPLINE_CURVE ( 3, ( #2179, #4004, #8915, #2280 ),
 .UNSPECIFIED., .F., .F. ) 
 B_SPLINE_CURVE_WITH_KNOTS ( ( 4, 4 ),
 ( 2.284520705739659263, 2.356010155625179348 ),
 .UNSPECIFIED. ) 
 CURVE ( )  GEOMETRIC_REPRESENTATION_ITEM ( )  RATIONAL_B_SPLINE_CURVE ( ( 1.000000000000000000, 0.9995741502243209453, 0.9995741502243209453, 1.000000000000000000 ) ) 
 REPRESENTATION_ITEM ( '' )  );
#1615 = ORIENTED_EDGE ( 'NONE', *, *, #3849, .F. ) ;
#1616 = AXIS2_PLACEMENT_3D ( 'NONE', #8394, #9070, #670 ) ;
#1617 = CARTESIAN_POINT ( 'NONE',  ( 10.19839929293505953, 0.4062499990440845421, -24.62111388750000174 ) ) ;
#1618 = DIRECTION ( 'NONE',  ( 0.000000000000000000, -2.775557561562887961E-17, -1.000000000000000000 ) ) ;
#1619 = CIRCLE ( 'NONE', #8151, 6.000000000000000888 ) ;
#1620 = CARTESIAN_POINT ( 'NONE',  ( -25.00000000000000000, 2.049999998088169129, -10.35533905932738108 ) ) ;
#1621 = LINE ( 'NONE', #3475, #5872 ) ;
#1622 = DIRECTION ( 'NONE',  ( -0.000000000000000000, -1.000000000000000000, -0.000000000000000000 ) ) ;
#1623 = EDGE_CURVE ( 'NONE', #10846, #3100, #2615, .T. ) ;
#1624 = CARTESIAN_POINT ( 'NONE',  ( 24.62111388749999463, 1.156249999044084431, 10.19839929293507730 ) ) ;
#1625 = DIRECTION ( 'NONE',  ( 0.000000000000000000, 1.502202555303639631E-16, 1.000000000000000000 ) ) ;
#1626 = ORIENTED_EDGE ( 'NONE', *, *, #2584, .F. ) ;
#1627 = VECTOR ( 'NONE', #3915, 1000.000000000000000 ) ;
#1628 = ORIENTED_EDGE ( 'NONE', *, *, #9519, .T. ) ;
#1629 = EDGE_LOOP ( 'NONE', ( #7601, #1408 ) ) ;
#1630 = VERTEX_POINT ( 'NONE', #6074 ) ;
#1631 = CIRCLE ( 'NONE', #10466, 0.1000000000000002554 ) ;
#1632 = ORIENTED_EDGE ( 'NONE', *, *, #1723, .T. ) ;
#1633 = VECTOR ( 'NONE', #10042, 1000.000000000000000 ) ;
#1634 = AXIS2_PLACEMENT_3D ( 'NONE', #5503, #2126, #5669 ) ;
#1635 = LINE ( 'NONE', #5020, #6567 ) ;
#1636 = CYLINDRICAL_SURFACE ( 'NONE', #6781, 4.500000000000000888 ) ;
#1637 = CARTESIAN_POINT ( 'NONE',  ( 0.000000000000000000, 10.00000000000000355, 0.000000000000000000 ) ) ;
#1638 = PLANE ( 'NONE',  #6593 ) ;
#1639 = CARTESIAN_POINT ( 'NONE',  ( 24.99258498528540429, 4.999999999999999112, 0.7093093681917175264 ) ) ;
#1640 =( GEOMETRIC_REPRESENTATION_CONTEXT ( 3 ) GLOBAL_UNCERTAINTY_ASSIGNED_CONTEXT ( ( #623 ) ) GLOBAL_UNIT_ASSIGNED_CONTEXT ( ( #723, #5751, #9996 ) ) REPRESENTATION_CONTEXT ( 'NONE', 'WORKASPACE' ) );
#1641 = CIRCLE ( 'NONE', #4499, 2.999999999999998224 ) ;
#1642 = VERTEX_POINT ( 'NONE', #8656 ) ;
#1643 = AXIS2_PLACEMENT_3D ( 'NONE', #3566, #4536, #5409 ) ;
#1644 = DIRECTION ( 'NONE',  ( -0.2500000000000009992, 0.8660254037844380415, 0.4330127018922199089 ) ) ;
#1645 = DIRECTION ( 'NONE',  ( 0.000000000000000000, 0.000000000000000000, 1.000000000000000000 ) ) ;
#1646 = CARTESIAN_POINT ( 'NONE',  ( -10.35533905932735621, 4.687500000000000888, 25.00000000000003197 ) ) ;
#1647 = FACE_OUTER_BOUND ( 'NONE', #4376, .T. ) ;
#1648 = DIRECTION ( 'NONE',  ( 0.000000000000000000, -2.775557561562888270E-17, -1.000000000000000000 ) ) ;
#1649 = PRODUCT_CONTEXT ( 'NONE', #4853, 'mechanical' ) ;
#1650 = FACE_OUTER_BOUND ( 'NONE', #9279, .T. ) ;
#1651 = CIRCLE ( 'NONE', #1150, 7.500000000000000888 ) ;
#1652 = CARTESIAN_POINT ( 'NONE',  ( -10.35533905932737220, 1.687500000000000222, 25.00000000000001421 ) ) ;
#1653 = CARTESIAN_POINT ( 'NONE',  ( 17.40975659021752620, 3.093749999044084653, 17.40975659021753330 ) ) ;
#1654 = CONICAL_SURFACE ( 'NONE', #4677, 2.000000000000000000, 1.029744258676657198 ) ;
#1655 = ORIENTED_EDGE ( 'NONE', *, *, #738, .F. ) ;
#1656 = ADVANCED_FACE ( 'NONE', ( #5950 ), #9433, .F. ) ;
#1657 = EDGE_CURVE ( 'NONE', #3713, #856, #7957, .T. ) ;
#1658 = VERTEX_POINT ( 'NONE', #7012 ) ;
#1659 = CARTESIAN_POINT ( 'NONE',  ( -10.19839929293505776, 4.706249999044084475, -24.62111388750000174 ) ) ;
#1660 = FACE_BOUND ( 'NONE', #22, .T. ) ;
#1661 = CARTESIAN_POINT ( 'NONE',  ( 10.19839929293506486, 5.206249999044084475, 24.62111388749999819 ) ) ;
#1662 = CARTESIAN_POINT ( 'NONE',  ( -7.000000000000002665, 10.00000000000000355, 0.4999999999999267253 ) ) ;
#1663 = ORIENTED_EDGE ( 'NONE', *, *, #8734, .F. ) ;
#1664 = CARTESIAN_POINT ( 'NONE',  ( -1.499999999999997780, 6.975000000000008527, 6.505213034913026604E-16 ) ) ;
#1665 = FILL_AREA_STYLE ('',( #10894 ) ) ;
#1666 = ADVANCED_FACE ( 'NONE', ( #6839 ), #5249, .T. ) ;
#1667 = DIRECTION ( 'NONE',  ( 0.000000000000000000, 0.000000000000000000, 1.000000000000000000 ) ) ;
#1668 = CARTESIAN_POINT ( 'NONE',  ( -3.058047309050066165, 19.03096903053433309, 6.296693311223885203 ) ) ;
#1669 = DIRECTION ( 'NONE',  ( 0.000000000000000000, 1.000000000000000000, 0.000000000000000000 ) ) ;
#1670 = DIRECTION ( 'NONE',  ( 0.000000000000000000, -0.000000000000000000, 1.000000000000000000 ) ) ;
#1671 = VERTEX_POINT ( 'NONE', #5196 ) ;
#1672 = EDGE_CURVE ( 'NONE', #6934, #10217, #2556, .T. ) ;
#1673 = VERTEX_POINT ( 'NONE', #210 ) ;
#1674 = ORIENTED_EDGE ( 'NONE', *, *, #5774, .F. ) ;
#1675 = DIRECTION ( 'NONE',  ( -0.000000000000000000, -1.000000000000000000, -0.000000000000000000 ) ) ;
#1676 = EDGE_CURVE ( 'NONE', #7970, #10189, #9176, .T. ) ;
#1677 = CARTESIAN_POINT ( 'NONE',  ( 24.62111388750000174, 3.456249999044084920, -10.19839929293505776 ) ) ;
#1678 = CARTESIAN_POINT ( 'NONE',  ( -17.40975659021753330, 1.843749999044084653, 17.40975659021752975 ) ) ;
#1679 = SURFACE_STYLE_USAGE ( .BOTH. , #9957 ) ;
#1680 = EDGE_CURVE ( 'NONE', #7784, #10524, #986, .T. ) ;
#1681 = CARTESIAN_POINT ( 'NONE',  ( 14.00000000000000533, 2.449293598294706907E-16, -2.000000000000000000 ) ) ;
#1682 = CARTESIAN_POINT ( 'NONE',  ( -7.874999999999821476, 28.00000000000000000, 13.63990010960501031 ) ) ;
#1683 = CARTESIAN_POINT ( 'NONE',  ( -24.62111388750000174, 3.718749999044084653, -3.015216831376932151E-15 ) ) ;
#1684 = LINE ( 'NONE', #9355, #8514 ) ;
#1685 = EDGE_LOOP ( 'NONE', ( #2047, #6952, #2247, #8218 ) ) ;
#1686 = ORIENTED_EDGE ( 'NONE', *, *, #7898, .T. ) ;
#1687 = ORIENTED_EDGE ( 'NONE', *, *, #1197, .T. ) ;
#1688 = ORIENTED_EDGE ( 'NONE', *, *, #5712, .F. ) ;
#1689 = ORIENTED_EDGE ( 'NONE', *, *, #8064, .T. ) ;
#1690 = DIRECTION ( 'NONE',  ( 0.000000000000000000, 0.000000000000000000, -1.000000000000000000 ) ) ;
#1691 = DIRECTION ( 'NONE',  ( 0.000000000000000000, 1.000000000000000000, 0.000000000000000000 ) ) ;
#1692 = DIRECTION ( 'NONE',  ( -0.000000000000000000, 1.000000000000000000, 0.000000000000000000 ) ) ;
#1693 = DIRECTION ( 'NONE',  ( 0.000000000000000000, 0.000000000000000000, -1.000000000000000000 ) ) ;
#1694 = FACE_OUTER_BOUND ( 'NONE', #4531, .T. ) ;
#1695 = VERTEX_POINT ( 'NONE', #10321 ) ;
#1696 = EDGE_CURVE ( 'NONE', #3821, #2862, #3161, .T. ) ;
#1697 = CARTESIAN_POINT ( 'NONE',  ( 0.000000000000000000, 0.000000000000000000, 0.000000000000000000 ) ) ;
#1698 = FILL_AREA_STYLE_COLOUR ( '', #4075 ) ;
#1699 = CARTESIAN_POINT ( 'NONE',  ( 0.000000000000000000, 0.000000000000000000, 0.000000000000000000 ) ) ;
#1700 = ORIENTED_EDGE ( 'NONE', *, *, #2592, .T. ) ;
#1701 = DIRECTION ( 'NONE',  ( -0.000000000000000000, -1.000000000000000000, -0.000000000000000000 ) ) ;
#1702 = DIRECTION ( 'NONE',  ( -0.000000000000000000, 1.000000000000000000, -0.000000000000000000 ) ) ;
#1703 = CARTESIAN_POINT ( 'NONE',  ( -17.67766952966369232, 5.237499998088169129, 17.67766952966368876 ) ) ;
#1704 = DIRECTION ( 'NONE',  ( -0.000000000000000000, 1.000000000000000000, -0.000000000000000000 ) ) ;
#1705 = ORIENTED_EDGE ( 'NONE', *, *, #4329, .F. ) ;
#1706 = CARTESIAN_POINT ( 'NONE',  ( -24.62111388750000884, 1.956249999044084475, 10.19839929293505421 ) ) ;
#1707 = DIRECTION ( 'NONE',  ( -0.8660254037844361541, 0.000000000000000000, 0.5000000000000042188 ) ) ;
#1708 = CARTESIAN_POINT ( 'NONE',  ( -10.19839929293507552, 3.906249999044085097, 24.62111388749999463 ) ) ;
#1709 = DIRECTION ( 'NONE',  ( -1.000000000000000000, 0.000000000000000000, 3.708321773340234242E-15 ) ) ;
#1710 = ORIENTED_EDGE ( 'NONE', *, *, #3464, .T. ) ;
#1711 = DIRECTION ( 'NONE',  ( 0.000000000000000000, 0.000000000000000000, -1.000000000000000000 ) ) ;
#1712 =( NAMED_UNIT ( * ) PLANE_ANGLE_UNIT ( ) SI_UNIT ( $, .RADIAN. ) );
#1713 = DIRECTION ( 'NONE',  ( 0.000000000000000000, -2.775557561562888270E-17, -1.000000000000000000 ) ) ;
#1714 = VECTOR ( 'NONE', #1182, 1000.000000000000114 ) ;
#1715 = EDGE_CURVE ( 'NONE', #6058, #7041, #5359, .T. ) ;
#1716 = CARTESIAN_POINT ( 'NONE',  ( 25.00000000000000000, 1.674999998088169351, -10.35533905932737753 ) ) ;
#1717 = CARTESIAN_POINT ( 'NONE',  ( 0.000000000000000000, 85.00000000000000000, -25.00000000000000000 ) ) ;
#1718 = DIRECTION ( 'NONE',  ( 0.000000000000000000, 0.4999999999999992228, -0.8660254037844391517 ) ) ;
#1719 = COLOUR_RGB ( '', 0.08235294, 0.09019608, 0.10196078) ;
#1720 = VERTEX_POINT ( 'NONE', #91 ) ;
#1721 = ORIENTED_EDGE ( 'NONE', *, *, #4770, .F. ) ;
#1722 = ORIENTED_EDGE ( 'NONE', *, *, #1203, .F. ) ;
#1723 = EDGE_CURVE ( 'NONE', #5890, #9754, #7660, .T. ) ;
#1724 = CONICAL_SURFACE ( 'NONE', #6487, 1.610000000000003872, 1.047197551196600518 ) ;
#1725 = UNCERTAINTY_MEASURE_WITH_UNIT (LENGTH_MEASURE( 1.000000000000000082E-05 ), #9113, 'distance_accuracy_value', 'NONE');
#1726 = CARTESIAN_POINT ( 'NONE',  ( 3.418204983771598122E-15, -55.00000000000000000, -27.91176187412963117 ) ) ;
#1727 = CARTESIAN_POINT ( 'NONE',  ( 17.40975659021752620, 3.268749999044084475, 17.40975659021753330 ) ) ;
#1728 = DIRECTION ( 'NONE',  ( 0.000000000000000000, 0.000000000000000000, 1.000000000000000000 ) ) ;
#1729 = CARTESIAN_POINT ( 'NONE',  ( 10.35533905932738286, 0.8125000000000001110, 24.99999999999999645 ) ) ;
#1730 =( LENGTH_UNIT ( ) NAMED_UNIT ( * ) SI_UNIT ( .MILLI., .METRE. ) );
#1731 = PRESENTATION_LAYER_ASSIGNMENT (  '', '', ( #1029 ) ) ;
#1732 = EDGE_CURVE ( 'NONE', #9229, #2686, #4962, .T. ) ;
#1733 = DIRECTION ( 'NONE',  ( 0.8660254037844382635, 0.5000000000000004441, 0.000000000000000000 ) ) ;
#1734 = CARTESIAN_POINT ( 'NONE',  ( -15.60400172474278158, 25.00000000000000000, -12.47307621135316680 ) ) ;
#1735 = VECTOR ( 'NONE', #5585, 1000.000000000000000 ) ;
#1736 = CARTESIAN_POINT ( 'NONE',  ( 10.35533905932738286, 1.812500000000000222, 24.99999999999999645 ) ) ;
#1737 = CARTESIAN_POINT ( 'NONE',  ( -19.75000000000003197, 25.00000000000000000, -2.999999999999789946 ) ) ;
#1738 = EDGE_LOOP ( 'NONE', ( #1366, #5245 ) ) ;
#1739 = ORIENTED_EDGE ( 'NONE', *, *, #5885, .T. ) ;
#1740 = ORIENTED_EDGE ( 'NONE', *, *, #3963, .T. ) ;
#1741 = EDGE_CURVE ( 'NONE', #5725, #3717, #1451, .T. ) ;
#1742 = CYLINDRICAL_SURFACE ( 'NONE', #7907, 6.000000000000000888 ) ;
#1743 = VECTOR ( 'NONE', #9170, 1000.000000000000000 ) ;
#1744 = DIRECTION ( 'NONE',  ( 0.000000000000000000, 0.000000000000000000, -1.000000000000000000 ) ) ;
#1745 = ORIENTED_EDGE ( 'NONE', *, *, #10441, .T. ) ;
#1746 = LINE ( 'NONE', #7490, #1473 ) ;
#1747 = DIRECTION ( 'NONE',  ( 0.000000000000000000, 0.000000000000000000, 1.000000000000000000 ) ) ;
#1748 =( BOUNDED_CURVE ( )  B_SPLINE_CURVE ( 2, ( #6391, #9845, #10685, #3838, #4731, #3043, #5608, #1350, #8725 ),
 .UNSPECIFIED., .F., .F. ) 
 B_SPLINE_CURVE_WITH_KNOTS ( ( 3, 2, 2, 2, 3 ),
 ( 0.8500000000000000888, 0.8750000000000001110, 0.9000000000000001332, 0.9250000000000001554, 0.9500000000000000666 ),
 .UNSPECIFIED. ) 
 CURVE ( )  GEOMETRIC_REPRESENTATION_ITEM ( )  RATIONAL_B_SPLINE_CURVE ( ( 0.9999999999999996669, 0.9238795325112870716, 1.000000000000000000, 0.9238795325112867385, 1.000000000000000000, 0.9238795325112867385, 1.000000000000000000, 0.9238795325112864054, 1.000000000000000444 ) ) 
 REPRESENTATION_ITEM ( '' )  );
#1749 = DIRECTION ( 'NONE',  ( -0.000000000000000000, 1.000000000000000000, -0.000000000000000000 ) ) ;
#1750 = DIRECTION ( 'NONE',  ( -0.000000000000000000, -1.000000000000000000, -0.000000000000000000 ) ) ;
#1751 = CARTESIAN_POINT ( 'NONE',  ( 18.79565575497285224, 5.000000000000000000, 16.19935794129608908 ) ) ;
#1752 = EDGE_CURVE ( 'NONE', #2032, #917, #8974, .T. ) ;
#1753 = ORIENTED_EDGE ( 'NONE', *, *, #6602, .F. ) ;
#1754 = CARTESIAN_POINT ( 'NONE',  ( 1.530808498934191521E-15, 1.862499998088169129, -25.00000000000000000 ) ) ;
#1755 = ORIENTED_EDGE ( 'NONE', *, *, #5501, .T. ) ;
#1756 = DIRECTION ( 'NONE',  ( 0.000000000000000000, -2.775557561562888270E-17, -1.000000000000000000 ) ) ;
#1757 = DIRECTION ( 'NONE',  ( -0.000000000000000000, 0.000000000000000000, 1.000000000000000000 ) ) ;
#1758 = VECTOR ( 'NONE', #8068, 999.9999999999998863 ) ;
#1759 = LINE ( 'NONE', #6132, #1365 ) ;
#1760 = DIRECTION ( 'NONE',  ( 0.000000000000000000, 1.000000000000000000, 0.000000000000000000 ) ) ;
#1761 = PLANE ( 'NONE',  #3883 ) ;
#1762 = CONTEXT_DEPENDENT_SHAPE_REPRESENTATION ( #3119, #85 ) ;
#1763 = DIRECTION ( 'NONE',  ( 0.000000000000000000, -1.000000000000000000, 0.000000000000000000 ) ) ;
#1764 = AXIS2_PLACEMENT_3D ( 'NONE', #3085, #4101, #3994 ) ;
#1765 = VERTEX_POINT ( 'NONE', #3843 ) ;
#1766 = AXIS2_PLACEMENT_3D ( 'NONE', #9474, #2825, #10304 ) ;
#1767 = CARTESIAN_POINT ( 'NONE',  ( 5.978755702618553158, 19.66631150450991683, -3.644491357022503930 ) ) ;
#1768 = CARTESIAN_POINT ( 'NONE',  ( 19.74999999999998934, -0.001000000000001000089, -3.000000000000067946 ) ) ;
#1769 = ORIENTED_EDGE ( 'NONE', *, *, #250, .T. ) ;
#1770 = EDGE_LOOP ( 'NONE', ( #121, #7110, #7664, #5985 ) ) ;
#1771 = AXIS2_PLACEMENT_3D ( 'NONE', #7914, #2808, #6207 ) ;
#1772 = CARTESIAN_POINT ( 'NONE',  ( 17.40975659021752975, 4.518749999044084475, -17.40975659021752975 ) ) ;
#1773 = PLANE ( 'NONE',  #8825 ) ;
#1774 = CARTESIAN_POINT ( 'NONE',  ( 1.400000000000001910, 0.000000000000000000, 0.000000000000000000 ) ) ;
#1775 = DIRECTION ( 'NONE',  ( -1.000000000000000000, 0.000000000000000000, -1.047444401652940007E-14 ) ) ;
#1776 = CARTESIAN_POINT ( 'NONE',  ( 0.000000000000000000, 7.000000000000003553, -2.149999999999999911 ) ) ;
#1777 = DIRECTION ( 'NONE',  ( 1.000000000000000000, 0.000000000000000000, 0.000000000000000000 ) ) ;
#1778 = CARTESIAN_POINT ( 'NONE',  ( -25.00000000000000000, 1.049999998088169129, -10.35533905932738108 ) ) ;
#1779 = CARTESIAN_POINT ( 'NONE',  ( 10.31217782649109971, 10.00000000000000355, -6.531088913245519656 ) ) ;
#1780 = CARTESIAN_POINT ( 'NONE',  ( -2.999999999999996447, 25.00000000000000000, 19.75000000000000000 ) ) ;
#1781 = VECTOR ( 'NONE', #8968, 1000.000000000000000 ) ;
#1782 = ORIENTED_EDGE ( 'NONE', *, *, #1321, .F. ) ;
#1783 = EDGE_LOOP ( 'NONE', ( #5615, #9402, #2481, #1034, #6737 ) ) ;
#1784 = ADVANCED_FACE ( 'NONE', ( #369 ), #3334, .F. ) ;
#1785 = CYLINDRICAL_SURFACE ( 'NONE', #4035, 25.00000000000000000 ) ;
#1786 = CARTESIAN_POINT ( 'NONE',  ( 24.62111388750000174, 3.393749999044084475, 0.000000000000000000 ) ) ;
#1787 = CARTESIAN_POINT ( 'NONE',  ( 3.058047309049977791, 19.03096903053433309, 6.296693311223928724 ) ) ;
#1788 = AXIS2_PLACEMENT_3D ( 'NONE', #5383, #9670, #2052 ) ;
#1789 = CARTESIAN_POINT ( 'NONE',  ( 1.507608415688466075E-15, 2.643749999044084920, -24.62111388750000174 ) ) ;
#1790 = CARTESIAN_POINT ( 'NONE',  ( 17.67766952966369232, 1.125000000000000222, -17.67766952966369232 ) ) ;
#1791 = VECTOR ( 'NONE', #7301, 1000.000000000000000 ) ;
#1792 = EDGE_LOOP ( 'NONE', ( #9713, #6544 ) ) ;
#1793 = LINE ( 'NONE', #2599, #4744 ) ;
#1794 = CARTESIAN_POINT ( 'NONE',  ( 4.895565917430008795, 5.000000000000001776, 24.12949820052922334 ) ) ;
#1795 = CARTESIAN_POINT ( 'NONE',  ( -10.35533905932737575, 2.312500000000000888, -25.00000000000000000 ) ) ;
#1796 = CARTESIAN_POINT ( 'NONE',  ( 1.507608415688466075E-15, 4.468749999044084653, -24.62111388750000174 ) ) ;
#1797 = CARTESIAN_POINT ( 'NONE',  ( -19.75000000000003197, 28.00000000000000000, -2.999999999999789946 ) ) ;
#1798 = ORIENTED_EDGE ( 'NONE', *, *, #6507, .F. ) ;
#1799 = ORIENTED_EDGE ( 'NONE', *, *, #10098, .T. ) ;
#1800 = EDGE_LOOP ( 'NONE', ( #5256, #9523, #3633, #4040 ) ) ;
#1801 = VECTOR ( 'NONE', #7530, 1000.000000000000114 ) ;
#1802 = ADVANCED_FACE ( 'NONE', ( #2125 ), #7260, .T. ) ;
#1803 = EDGE_CURVE ( 'NONE', #1671, #7292, #4784, .T. ) ;
#1804 = DIRECTION ( 'NONE',  ( 0.000000000000000000, 1.000000000000000000, 0.000000000000000000 ) ) ;
#1805 = CARTESIAN_POINT ( 'NONE',  ( -25.00000000000001066, 4.174999998088169129, 10.35533905932737397 ) ) ;
#1806 = CARTESIAN_POINT ( 'NONE',  ( -6.531088913245408634, 10.00000000000000355, -10.31217782649116188 ) ) ;
#1807 = EDGE_CURVE ( 'NONE', #9105, #9832, #9360, .T. ) ;
#1808 = DIRECTION ( 'NONE',  ( 0.4999999999999980016, 0.000000000000000000, 0.8660254037844398178 ) ) ;
#1809 = AXIS2_PLACEMENT_3D ( 'NONE', #6300, #1014, #8778 ) ;
#1810 = DIRECTION ( 'NONE',  ( -0.000000000000000000, 1.000000000000000000, -0.000000000000000000 ) ) ;
#1811 = DIRECTION ( 'NONE',  ( 0.000000000000000000, 0.000000000000000000, 1.000000000000000000 ) ) ;
#1812 = DIRECTION ( 'NONE',  ( 0.5000000000000012212, -0.000000000000000000, 0.8660254037844380415 ) ) ;
#1813 = ORIENTED_EDGE ( 'NONE', *, *, #10030, .T. ) ;
#1814 = EDGE_CURVE ( 'NONE', #2818, #8744, #9749, .T. ) ;
#1815 = CIRCLE ( 'NONE', #7988, 2.999999999999997335 ) ;
#1816 = VERTEX_POINT ( 'NONE', #8919 ) ;
#1817 = VECTOR ( 'NONE', #6504, 1000.000000000000114 ) ;
#1818 = LINE ( 'NONE', #10929, #9680 ) ;
#1819 = FACE_OUTER_BOUND ( 'NONE', #7522, .T. ) ;
#1820 = CARTESIAN_POINT ( 'NONE',  ( 0.2251666049839524120, 0.000000000000000000, 0.000000000000000000 ) ) ;
#1821 = CARTESIAN_POINT ( 'NONE',  ( 10.19839929293506486, 1.206249999044084698, 24.62111388749999819 ) ) ;
#1822 =( BOUNDED_CURVE ( )  B_SPLINE_CURVE ( 2, ( #10813, #10143, #4235, #5074, #9193 ),
 .UNSPECIFIED., .F., .F. ) 
 B_SPLINE_CURVE_WITH_KNOTS ( ( 3, 2, 3 ),
 ( 0.9500000000000000666, 0.9750000000000000888, 1.000000000000000000 ),
 .UNSPECIFIED. ) 
 CURVE ( )  GEOMETRIC_REPRESENTATION_ITEM ( )  RATIONAL_B_SPLINE_CURVE ( ( 0.9999999999999996669, 0.9238795325112870716, 1.000000000000000000, 0.9238795325112867385, 1.000000000000000000 ) ) 
 REPRESENTATION_ITEM ( '' )  );
#1823 = CIRCLE ( 'NONE', #7994, 5.100000000000006750 ) ;
#1824 = CARTESIAN_POINT ( 'NONE',  ( 19.75000000000001066, -0.001000000000001000089, 2.999999999999927613 ) ) ;
#1825 = AXIS2_PLACEMENT_3D ( 'NONE', #4036, #4920, #5743 ) ;
#1826 = ADVANCED_FACE ( 'NONE', ( #425 ), #7213, .T. ) ;
#1827 = CARTESIAN_POINT ( 'NONE',  ( -3.499999999999921840, 20.00000000000000355, -6.062177826491114807 ) ) ;
#1828 = CARTESIAN_POINT ( 'NONE',  ( 1.530808498934191521E-15, 4.862499998088169129, -25.00000000000000000 ) ) ;
#1829 = DIRECTION ( 'NONE',  ( -0.5000000000000012212, 0.000000000000000000, -0.8660254037844380415 ) ) ;
#1830 = VECTOR ( 'NONE', #4405, 1000.000000000000114 ) ;
#1831 = VECTOR ( 'NONE', #1810, 1000.000000000000000 ) ;
#1832 = CARTESIAN_POINT ( 'NONE',  ( -17.40975659021752975, 3.768749999044084475, -17.40975659021752975 ) ) ;
#1833 = CARTESIAN_POINT ( 'NONE',  ( 82.32050807568876394, 92.28203230275514102, 0.000000000000000000 ) ) ;
#1834 = CARTESIAN_POINT ( 'NONE',  ( 24.62111388750000174, 5.218749999044084653, 0.000000000000000000 ) ) ;
#1835 = DIRECTION ( 'NONE',  ( 0.000000000000000000, 0.000000000000000000, 1.000000000000000000 ) ) ;
#1836 = ORIENTED_EDGE ( 'NONE', *, *, #9427, .T. ) ;
#1837 = CARTESIAN_POINT ( 'NONE',  ( -15.75000000000003553, 25.00000000000000000, -2.999999999999832578 ) ) ;
#1838 = CARTESIAN_POINT ( 'NONE',  ( -20.63749999999999574, 0.000000000000000000, 0.000000000000000000 ) ) ;
#1839 = LINE ( 'NONE', #173, #7737 ) ;
#1840 = AXIS2_PLACEMENT_3D ( 'NONE', #2183, #9848, #5666 ) ;
#1841 = DIRECTION ( 'NONE',  ( 2.168404344971010347E-16, -0.000000000000000000, 1.000000000000000000 ) ) ;
#1842 = CARTESIAN_POINT ( 'NONE',  ( 10.35533905932738286, 3.812500000000000000, 24.99999999999999645 ) ) ;
#1843 = VERTEX_POINT ( 'NONE', #7167 ) ;
#1844 = EDGE_LOOP ( 'NONE', ( #2368, #5001 ) ) ;
#1845 = CARTESIAN_POINT ( 'NONE',  ( 0.000000000000000000, 0.000000000000000000, -25.00000000000000000 ) ) ;
#1846 = CARTESIAN_POINT ( 'NONE',  ( 24.62111388749999463, 3.331249999044084920, 10.19839929293507730 ) ) ;
#1847 = CARTESIAN_POINT ( 'NONE',  ( -10.81217782649101977, 10.00000000000000355, -5.665063509461230495 ) ) ;
#1848 = CARTESIAN_POINT ( 'NONE',  ( -17.67766952966369232, 4.237499998088169129, 17.67766952966368876 ) ) ;
#1849 = CARTESIAN_POINT ( 'NONE',  ( -4.592425496802574367E-15, 0.7500000000000000000, 25.00000000000000000 ) ) ;
#1850 = CARTESIAN_POINT ( 'NONE',  ( 7.874999999999916511, -0.001000000000001000089, -13.63990010960495702 ) ) ;
#1851 = VERTEX_POINT ( 'NONE', #10530 ) ;
#1852 = CARTESIAN_POINT ( 'NONE',  ( 1.530808498934191521E-15, 2.862499998088169573, -25.00000000000000000 ) ) ;
#1853 = CARTESIAN_POINT ( 'NONE',  ( -6.062177826491100596, 20.00000000000000355, 3.499999999999942712 ) ) ;
#1854 = LINE ( 'NONE', #5289, #5843 ) ;
#1855 = DIRECTION ( 'NONE',  ( 0.4999999999999887312, 0.000000000000000000, -0.8660254037844451469 ) ) ;
#1856 = DIRECTION ( 'NONE',  ( 0.8660254037844382635, 0.5000000000000004441, 0.000000000000000000 ) ) ;
#1857 = VERTEX_POINT ( 'NONE', #577 ) ;
#1858 = VERTEX_POINT ( 'NONE', #3959 ) ;
#1859 = ORIENTED_EDGE ( 'NONE', *, *, #8200, .F. ) ;
#1860 = VERTEX_POINT ( 'NONE', #6291 ) ;
#1861 = CARTESIAN_POINT ( 'NONE',  ( -4.592425496802574367E-15, 3.362499998088169129, 25.00000000000000000 ) ) ;
#1862 = FACE_OUTER_BOUND ( 'NONE', #4884, .T. ) ;
#1863 = ORIENTED_EDGE ( 'NONE', *, *, #2250, .F. ) ;
#1864 = DIRECTION ( 'NONE',  ( -0.000000000000000000, 1.000000000000000000, -0.000000000000000000 ) ) ;
#1865 = CARTESIAN_POINT ( 'NONE',  ( 27.32050807568876749, 100.0000000000000142, 5.000000000000000000 ) ) ;
#1866 = LINE ( 'NONE', #5248, #3210 ) ;
#1867 = EDGE_CURVE ( 'NONE', #4439, #9521, #3049, .T. ) ;
#1868 = DIRECTION ( 'NONE',  ( 0.000000000000000000, -2.775557561562887961E-17, -1.000000000000000000 ) ) ;
#1869 = DIRECTION ( 'NONE',  ( 0.000000000000000000, 1.000000000000000000, 0.000000000000000000 ) ) ;
#1870 = CARTESIAN_POINT ( 'NONE',  ( 0.2499999999999990286, 0.000000000000000000, 0.4330127018922199644 ) ) ;
#1871 = ORIENTED_EDGE ( 'NONE', *, *, #5325, .F. ) ;
#1872 = ADVANCED_FACE ( 'NONE', ( #2995 ), #2940, .T. ) ;
#1873 = ORIENTED_EDGE ( 'NONE', *, *, #1623, .T. ) ;
#1874 = DIRECTION ( 'NONE',  ( -0.000000000000000000, -0.000000000000000000, -1.000000000000000000 ) ) ;
#1875 = CARTESIAN_POINT ( 'NONE',  ( 0.000000000000000000, 85.00000000000000000, 0.000000000000000000 ) ) ;
#1876 = CARTESIAN_POINT ( 'NONE',  ( 17.40975659021752975, 1.518749999044084698, -17.40975659021752975 ) ) ;
#1877 = ORIENTED_EDGE ( 'NONE', *, *, #8898, .F. ) ;
#1878 = CARTESIAN_POINT ( 'NONE',  ( 9.875000000000023093, 28.00000000000000000, 17.10400172474264835 ) ) ;
#1879 = APPLICATION_PROTOCOL_DEFINITION ( 'draft international standard', 'automotive_design', 1998, #1046 ) ;
#1880 = DIRECTION ( 'NONE',  ( -0.6546536707079723127, -0.000000000000000000, 0.7559289460184587250 ) ) ;
#1881 = CARTESIAN_POINT ( 'NONE',  ( 17.10400172474261637, 28.00000000000000000, -9.875000000000085265 ) ) ;
#1882 = EDGE_CURVE ( 'NONE', #5496, #4908, #5613, .T. ) ;
#1883 = ADVANCED_FACE ( 'NONE', ( #5502 ), #5562, .T. ) ;
#1884 = CARTESIAN_POINT ( 'NONE',  ( -4.522825247065398226E-15, 4.143749999044083587, 24.62111388750000174 ) ) ;
#1885 = CARTESIAN_POINT ( 'NONE',  ( -4.592425496802574367E-15, 1.750000000000000000, 25.00000000000000000 ) ) ;
#1886 = CARTESIAN_POINT ( 'NONE',  ( -24.62111388750000884, 4.781249999044083765, 10.19839929293505421 ) ) ;
#1887 = CARTESIAN_POINT ( 'NONE',  ( -24.62111388750000174, 1.893749999044084475, -3.015216831376932151E-15 ) ) ;
#1888 = ORIENTED_EDGE ( 'NONE', *, *, #459, .F. ) ;
#1889 = DIRECTION ( 'NONE',  ( 0.8660254037844380415, 0.000000000000000000, -0.5000000000000012212 ) ) ;
#1890 =( LENGTH_UNIT ( ) NAMED_UNIT ( * ) SI_UNIT ( .MILLI., .METRE. ) );
#1891 = PLANE ( 'NONE',  #10641 ) ;
#1892 = CARTESIAN_POINT ( 'NONE',  ( -17.40975659021752975, 0.5937499990440846531, -17.40975659021752975 ) ) ;
#1893 = CARTESIAN_POINT ( 'NONE',  ( 6.062177826491073063, 20.00000000000000355, -3.499999999999989786 ) ) ;
#1894 = CARTESIAN_POINT ( 'NONE',  ( -17.67766952966369232, 2.625000000000000000, 17.67766952966368876 ) ) ;
#1895 = ORIENTED_EDGE ( 'NONE', *, *, #6352, .F. ) ;
#1896 = EDGE_LOOP ( 'NONE', ( #9721, #7390 ) ) ;
#1897 = ADVANCED_FACE ( 'NONE', ( #4692 ), #10067, .T. ) ;
#1898 = PRESENTATION_LAYER_ASSIGNMENT (  '', '', ( #10362 ) ) ;
#1899 = CARTESIAN_POINT ( 'NONE',  ( 1.040834085586084257E-14, 90.00000000000001421, 0.000000000000000000 ) ) ;
#1900 = CARTESIAN_POINT ( 'NONE',  ( -24.62111388750000884, 3.956249999044084920, 10.19839929293505421 ) ) ;
#1901 = DIRECTION ( 'NONE',  ( 0.000000000000000000, 1.000000000000000000, 0.000000000000000000 ) ) ;
#1902 = CARTESIAN_POINT ( 'NONE',  ( 25.00000000000000000, 3.674999998088170017, -10.35533905932737753 ) ) ;
#1903 = CARTESIAN_POINT ( 'NONE',  ( -17.40975659021753330, 3.843749999044085097, 17.40975659021752975 ) ) ;
#1904 = CARTESIAN_POINT ( 'NONE',  ( 0.000000000000000000, 0.000000000000000000, 0.000000000000000000 ) ) ;
#1905 = LINE ( 'NONE', #10303, #10552 ) ;
#1906 = CYLINDRICAL_SURFACE ( 'NONE', #8650, 2.999999999999997780 ) ;
#1907 = FACE_OUTER_BOUND ( 'NONE', #6597, .T. ) ;
#1908 = CARTESIAN_POINT ( 'NONE',  ( 25.00000000000000000, 5.000000000000000000, 0.000000000000000000 ) ) ;
#1909 = CARTESIAN_POINT ( 'NONE',  ( -4.592425496802574367E-15, 3.362499998088169129, 25.00000000000000000 ) ) ;
#1910 = ORIENTED_EDGE ( 'NONE', *, *, #6520, .F. ) ;
#1911 = CIRCLE ( 'NONE', #10542, 6.999999999999997335 ) ;
#1912 = ORIENTED_EDGE ( 'NONE', *, *, #9089, .F. ) ;
#1913 = ORIENTED_EDGE ( 'NONE', *, *, #1752, .T. ) ;
#1914 = DIRECTION ( 'NONE',  ( 0.000000000000000000, 1.000000000000000000, 0.000000000000000000 ) ) ;
#1915 = COLOUR_RGB ( '', 0.31764706, 0.68627451, 0.89019608) ;
#1916 = AXIS2_PLACEMENT_3D ( 'NONE', #6310, #548, #4560 ) ;
#1917 = DIRECTION ( 'NONE',  ( 0.000000000000000000, 0.000000000000000000, -1.000000000000000000 ) ) ;
#1918 = ORIENTED_EDGE ( 'NONE', *, *, #7828, .F. ) ;
#1919 = CYLINDRICAL_SURFACE ( 'NONE', #7133, 2.999999999999999112 ) ;
#1920 = FACE_OUTER_BOUND ( 'NONE', #7536, .T. ) ;
#1921 = CARTESIAN_POINT ( 'NONE',  ( 0.000000000000000000, -55.00000000000000000, 0.000000000000000000 ) ) ;
#1922 = LINE ( 'NONE', #7778, #4446 ) ;
#1923 = CARTESIAN_POINT ( 'NONE',  ( -4.592425496802574367E-15, 1.750000000000000000, 25.00000000000000000 ) ) ;
#1924 = CARTESIAN_POINT ( 'NONE',  ( -24.62111388750000174, 3.831249999044084920, -10.19839929293506131 ) ) ;
#1925 = ORIENTED_EDGE ( 'NONE', *, *, #5459, .F. ) ;
#1926 = AXIS2_PLACEMENT_3D ( 'NONE', #10233, #71, #10174 ) ;
#1927 = ORIENTED_EDGE ( 'NONE', *, *, #4733, .F. ) ;
#1928 = EDGE_CURVE ( 'NONE', #4468, #7572, #3729, .T. ) ;
#1929 = EDGE_CURVE ( 'NONE', #8979, #2617, #2296, .T. ) ;
#1930 = CARTESIAN_POINT ( 'NONE',  ( 0.000000000000000000, 1.971681346627243419E-16, 1.610000000000003872 ) ) ;
#1931 = CARTESIAN_POINT ( 'NONE',  ( 12.47307621135333200, -0.001000000000001000089, 15.60400172474264835 ) ) ;
#1932 = CARTESIAN_POINT ( 'NONE',  ( 24.62111388750000174, 4.456249999044084475, -10.19839929293505776 ) ) ;
#1933 = EDGE_LOOP ( 'NONE', ( #9853, #3773, #3245, #7484, #8511, #7424 ) ) ;
#1934 = CARTESIAN_POINT ( 'NONE',  ( 0.000000000000000000, 7.000000000000003553, 12.77350269189627063 ) ) ;
#1935 = LINE ( 'NONE', #2084, #964 ) ;
#1936 = CARTESIAN_POINT ( 'NONE',  ( -15.60400172474251868, 28.00000000000000000, 12.47307621135349720 ) ) ;
#1937 = CARTESIAN_POINT ( 'NONE',  ( 10.19839929293506486, 4.031249999044083765, 24.62111388749999819 ) ) ;
#1938 = EDGE_CURVE ( 'NONE', #9084, #4561, #9589, .T. ) ;
#1939 = ORIENTED_EDGE ( 'NONE', *, *, #9085, .T. ) ;
#1940 = ADVANCED_FACE ( 'NONE', ( #194 ), #2768, .T. ) ;
#1941 = LINE ( 'NONE', #1273, #8795 ) ;
#1942 = CARTESIAN_POINT ( 'NONE',  ( 17.67766952966369232, 2.125000000000000000, -17.67766952966369232 ) ) ;
#1943 = CARTESIAN_POINT ( 'NONE',  ( 10.19839929293506486, 4.031249999044083765, 24.62111388749999819 ) ) ;
#1944 = AXIS2_PLACEMENT_3D ( 'NONE', #4338, #7926, #5175 ) ;
#1945 = LINE ( 'NONE', #3530, #6745 ) ;
#1946 = ORIENTED_EDGE ( 'NONE', *, *, #2141, .F. ) ;
#1947 = CARTESIAN_POINT ( 'NONE',  ( -25.00000000000000000, 1.049999998088169129, -10.35533905932738108 ) ) ;
#1948 =( NAMED_UNIT ( * ) SI_UNIT ( $, .STERADIAN. ) SOLID_ANGLE_UNIT ( ) );
#1949 = DIRECTION ( 'NONE',  ( 0.000000000000000000, 0.000000000000000000, 1.000000000000000000 ) ) ;
#1950 = CYLINDRICAL_SURFACE ( 'NONE', #5363, 2.999999999999997335 ) ;
#1951 = CARTESIAN_POINT ( 'NONE',  ( -10.35533905932737575, 0.9249999980881692396, -25.00000000000000000 ) ) ;
#1952 = EDGE_CURVE ( 'NONE', #3209, #4627, #372, .T. ) ;
#1953 = PRODUCT_DEFINITION_SHAPE ( 'NONE', 'NONE',  #6924 ) ;
#1954 = ORIENTED_EDGE ( 'NONE', *, *, #5712, .T. ) ;
#1955 = AXIS2_PLACEMENT_3D ( 'NONE', #7089, #3764, #2202 ) ;
#1956 = ORIENTED_EDGE ( 'NONE', *, *, #7453, .F. ) ;
#1957 = CIRCLE ( 'NONE', #6896, 24.91176187412963117 ) ;
#1958 =( BOUNDED_CURVE ( )  B_SPLINE_CURVE ( 2, ( #3890, #10574, #1349, #10627, #466, #421, #3042, #9793, #6389 ),
 .UNSPECIFIED., .F., .F. ) 
 B_SPLINE_CURVE_WITH_KNOTS ( ( 3, 2, 2, 2, 3 ),
 ( 0.05000000000000000278, 0.07500000000000001110, 0.1000000000000000194, 0.1250000000000000278, 0.1500000000000000222 ),
 .UNSPECIFIED. ) 
 CURVE ( )  GEOMETRIC_REPRESENTATION_ITEM ( )  RATIONAL_B_SPLINE_CURVE ( ( 1.000000000000000000, 0.9238795325112867385, 1.000000000000000000, 0.9238795325112867385, 1.000000000000000000, 0.9238795325112867385, 1.000000000000000000, 0.9238795325112866275, 1.000000000000000000 ) ) 
 REPRESENTATION_ITEM ( '' )  );
#1959 = ORIENTED_EDGE ( 'NONE', *, *, #3062, .T. ) ;
#1960 = EDGE_CURVE ( 'NONE', #3974, #5443, #9639, .T. ) ;
#1961 = CARTESIAN_POINT ( 'NONE',  ( 24.62111388750000174, 2.218749999044084653, 0.000000000000000000 ) ) ;
#1962 = DIRECTION ( 'NONE',  ( 1.000000000000000000, 0.000000000000000000, 0.000000000000000000 ) ) ;
#1963 = CARTESIAN_POINT ( 'NONE',  ( 25.00000000000000000, 2.612499998088169129, 0.000000000000000000 ) ) ;
#1964 = CARTESIAN_POINT ( 'NONE',  ( 25.00000000000000000, 0.06249999999999997224, -10.35533905932737753 ) ) ;
#1965 = CARTESIAN_POINT ( 'NONE',  ( -17.67766952966368876, 2.987499998088169129, -17.67766952966369232 ) ) ;
#1966 = AXIS2_PLACEMENT_3D ( 'NONE', #6342, #8091, #5453 ) ;
#1967 = VECTOR ( 'NONE', #5378, 1000.000000000000000 ) ;
#1968 = ADVANCED_FACE ( 'NONE', ( #10409 ), #2065, .F. ) ;
#1969 = LINE ( 'NONE', #9351, #5442 ) ;
#1970 = CARTESIAN_POINT ( 'NONE',  ( 7.276923788646575630, -0.001000000000001000089, -18.60400172474270519 ) ) ;
#1971 = CYLINDRICAL_SURFACE ( 'NONE', #1094, 25.00000000000000000 ) ;
#1972 = ADVANCED_FACE ( 'NONE', ( #8581 ), #1971, .T. ) ;
#1973 = CARTESIAN_POINT ( 'NONE',  ( -17.67766952966369232, 1.625000000000000222, 17.67766952966368876 ) ) ;
#1974 = CARTESIAN_POINT ( 'NONE',  ( -10.35533905932739174, 3.299999998088169129, 24.99999999999999289 ) ) ;
#1975 = ORIENTED_EDGE ( 'NONE', *, *, #9810, .T. ) ;
#1976 = VERTEX_POINT ( 'NONE', #7979 ) ;
#1977 = VECTOR ( 'NONE', #9787, 1000.000000000000114 ) ;
#1978 = LINE ( 'NONE', #7770, #4195 ) ;
#1979 = EDGE_CURVE ( 'NONE', #5812, #9541, #10066, .T. ) ;
#1980 = FACE_OUTER_BOUND ( 'NONE', #2514, .T. ) ;
#1981 = PLANE ( 'NONE',  #3197 ) ;
#1982 = CARTESIAN_POINT ( 'NONE',  ( 0.000000000000000000, 85.00000000000000000, 0.000000000000000000 ) ) ;
#1983 = DIRECTION ( 'NONE',  ( 0.000000000000000000, 0.000000000000000000, 1.000000000000000000 ) ) ;
#1984 = DIRECTION ( 'NONE',  ( 0.5000000000000101030, 0.000000000000000000, -0.8660254037844328234 ) ) ;
#1985 = CARTESIAN_POINT ( 'NONE',  ( 1.507608415688466075E-15, 3.643749999044084920, -24.62111388750000174 ) ) ;
#1986 = CIRCLE ( 'NONE', #4802, 25.00000000000000000 ) ;
#1987 = VERTEX_POINT ( 'NONE', #1241 ) ;
#1988 = VERTEX_POINT ( 'NONE', #3554 ) ;
#1989 = ORIENTED_EDGE ( 'NONE', *, *, #8416, .F. ) ;
#1990 = LINE ( 'NONE', #2225, #1781 ) ;
#1991 = DIRECTION ( 'NONE',  ( -0.000000000000000000, 1.000000000000000000, 0.000000000000000000 ) ) ;
#1992 = CARTESIAN_POINT ( 'NONE',  ( 10.19839929293505953, 2.581249999044084920, -24.62111388750000174 ) ) ;
#1993 = ORIENTED_EDGE ( 'NONE', *, *, #4111, .T. ) ;
#1994 = FACE_OUTER_BOUND ( 'NONE', #2153, .T. ) ;
#1995 = FACE_OUTER_BOUND ( 'NONE', #7039, .T. ) ;
#1996 = LINE ( 'NONE', #2087, #229 ) ;
#1997 = AXIS2_PLACEMENT_3D ( 'NONE', #1600, #4986, #2576 ) ;
#1998 = CIRCLE ( 'NONE', #8154, 0.1000000000000002554 ) ;
#1999 = VECTOR ( 'NONE', #4701, 1000.000000000000000 ) ;
#2000 = ORIENTED_EDGE ( 'NONE', *, *, #4111, .F. ) ;
#2001 = AXIS2_PLACEMENT_3D ( 'NONE', #8652, #7888, #5191 ) ;
#2002 = VECTOR ( 'NONE', #6089, 1000.000000000000000 ) ;
#2003 = CARTESIAN_POINT ( 'NONE',  ( 25.00000000000000000, 2.000000000000000000, 0.000000000000000000 ) ) ;
#2004 = CARTESIAN_POINT ( 'NONE',  ( -24.13837508890848227, 4.999999999999997335, -6.164697453113522130 ) ) ;
#2005 = DIRECTION ( 'NONE',  ( -0.000000000000000000, -0.000000000000000000, -1.000000000000000000 ) ) ;
#2006 = ORIENTED_EDGE ( 'NONE', *, *, #699, .F. ) ;
#2007 = CARTESIAN_POINT ( 'NONE',  ( -1.500000000000000444, 83.00000000000000000, 1.499999999999999778 ) ) ;
#2008 = CARTESIAN_POINT ( 'NONE',  ( -1.500000000000001332, 1.119140903701213403E-15, 7.399999999999999467 ) ) ;
#2009 = CIRCLE ( 'NONE', #7445, 6.750000000000007994 ) ;
#2010 = CARTESIAN_POINT ( 'NONE',  ( -17.40975659021752975, 1.593749999044084431, -17.40975659021752975 ) ) ;
#2011 = CARTESIAN_POINT ( 'NONE',  ( 25.00000000000000000, 0.3062499990440845643, 0.000000000000000000 ) ) ;
#2012 = EDGE_CURVE ( 'NONE', #4087, #5829, #3345, .T. ) ;
#2013 = PRESENTATION_LAYER_ASSIGNMENT (  '', '', ( #5521 ) ) ;
#2014 = AXIS2_PLACEMENT_3D ( 'NONE', #4180, #7777, #985 ) ;
#2015 = EDGE_LOOP ( 'NONE', ( #809, #5825, #3140, #9910 ) ) ;
#2016 = ORIENTED_EDGE ( 'NONE', *, *, #3973, .F. ) ;
#2017 = CONICAL_SURFACE ( 'NONE', #5011, 2.000000000000004441, 0.7853981633974496113 ) ;
#2018 = ADVANCED_FACE ( 'NONE', ( #4526, #8756 ), #356, .T. ) ;
#2019 = CARTESIAN_POINT ( 'NONE',  ( -17.40975659021753330, 4.843749999044083765, 17.40975659021752975 ) ) ;
#2020 = CARTESIAN_POINT ( 'NONE',  ( 17.40975659021752620, 4.268749999044085364, 17.40975659021753330 ) ) ;
#2021 = CARTESIAN_POINT ( 'NONE',  ( 25.00000000000000000, 2.674999998088169129, -10.35533905932737753 ) ) ;
#2022 = AXIS2_PLACEMENT_3D ( 'NONE', #3911, #530, #4800 ) ;
#2023 = CARTESIAN_POINT ( 'NONE',  ( -25.00000000000000000, 1.500000000000000000, -3.061616997868383043E-15 ) ) ;
#2024 = FACE_BOUND ( 'NONE', #9135, .T. ) ;
#2025 = LINE ( 'NONE', #3551, #3147 ) ;
#2026 = DIRECTION ( 'NONE',  ( 0.000000000000000000, -1.000000000000000000, 0.000000000000000000 ) ) ;
#2027 = DIRECTION ( 'NONE',  ( 0.000000000000000000, 1.000000000000000000, -0.000000000000000000 ) ) ;
#2028 = AXIS2_PLACEMENT_3D ( 'NONE', #6557, #8003, #8927 ) ;
#2029 = EDGE_CURVE ( 'NONE', #8291, #4468, #5329, .T. ) ;
#2030 = CARTESIAN_POINT ( 'NONE',  ( -12.47307621135311351, -0.001000000000001000089, 15.60400172474282599 ) ) ;
#2031 = ORIENTED_EDGE ( 'NONE', *, *, #9706, .T. ) ;
#2032 = VERTEX_POINT ( 'NONE', #8639 ) ;
#2033 = EDGE_CURVE ( 'NONE', #8288, #8662, #4463, .T. ) ;
#2034 = DIRECTION ( 'NONE',  ( 0.000000000000000000, 2.775557561562888270E-17, 1.000000000000000000 ) ) ;
#2035 = CARTESIAN_POINT ( 'NONE',  ( 24.62111388750000174, 0.2187499990440845699, 0.000000000000000000 ) ) ;
#2036 = CARTESIAN_POINT ( 'NONE',  ( -0.2500000000000050515, 0.000000000000000000, 0.4330127018922164117 ) ) ;
#2037 = CARTESIAN_POINT ( 'NONE',  ( 10.19839929293506486, 5.206249999044084475, 24.62111388749999819 ) ) ;
#2038 = VERTEX_POINT ( 'NONE', #7823 ) ;
#2039 = ADVANCED_FACE ( 'NONE', ( #1028 ), #252, .F. ) ;
#2040 = ORIENTED_EDGE ( 'NONE', *, *, #1867, .F. ) ;
#2041 = CARTESIAN_POINT ( 'NONE',  ( 24.62111388749999108, 3.331249999044084920, 10.19839929293507730 ) ) ;
#2042 = DIRECTION ( 'NONE',  ( 0.000000000000000000, 1.000000000000000000, 0.000000000000000000 ) ) ;
#2043 = CARTESIAN_POINT ( 'NONE',  ( 0.000000000000000000, 85.00000000000000000, 0.000000000000000000 ) ) ;
#2044 = CARTESIAN_POINT ( 'NONE',  ( 1.400000000000001910, 0.000000000000000000, 0.000000000000000000 ) ) ;
#2045 = CARTESIAN_POINT ( 'NONE',  ( 3.499999999999963141, 20.00000000000000355, 6.062177826491089050 ) ) ;
#2046 = VERTEX_POINT ( 'NONE', #3882 ) ;
#2047 = ORIENTED_EDGE ( 'NONE', *, *, #8553, .T. ) ;
#2048 = CARTESIAN_POINT ( 'NONE',  ( 12.13990010960493748, 25.00000000000000000, 10.47307621135328759 ) ) ;
#2049 = DIRECTION ( 'NONE',  ( -0.4999999999999888978, 0.000000000000000000, 0.8660254037844450359 ) ) ;
#2050 = CARTESIAN_POINT ( 'NONE',  ( 6.062177826491051746, 20.00000000000000355, 3.500000000000027089 ) ) ;
#2051 = EDGE_LOOP ( 'NONE', ( #8901, #2903, #8334, #2831 ) ) ;
#2052 = DIRECTION ( 'NONE',  ( 0.000000000000000000, 0.000000000000000000, 1.000000000000000000 ) ) ;
#2053 = LINE ( 'NONE', #1229, #4493 ) ;
#2054 = CARTESIAN_POINT ( 'NONE',  ( -24.62111388750000174, 4.718749999044084653, -3.015216831376932151E-15 ) ) ;
#2055 = DIRECTION ( 'NONE',  ( -0.000000000000000000, 1.000000000000000000, -0.000000000000000000 ) ) ;
#2056 = ORIENTED_EDGE ( 'NONE', *, *, #4452, .F. ) ;
#2057 = CARTESIAN_POINT ( 'NONE',  ( -24.62111388750000884, 2.781249999044085541, 10.19839929293505421 ) ) ;
#2058 = CARTESIAN_POINT ( 'NONE',  ( -17.40975659021753330, 3.018749999044084475, 17.40975659021752975 ) ) ;
#2059 = ADVANCED_FACE ( 'NONE', ( #5551 ), #3998, .T. ) ;
#2060 = CARTESIAN_POINT ( 'NONE',  ( -25.00000000000001421, 3.562500000000000444, 10.35533905932737397 ) ) ;
#2061 =( LENGTH_UNIT ( ) NAMED_UNIT ( * ) SI_UNIT ( .MILLI., .METRE. ) );
#2062 = CARTESIAN_POINT ( 'NONE',  ( -6.982120021884462346, 10.00000000000000355, -0.5000000000000731637 ) ) ;
#2063 = DIRECTION ( 'NONE',  ( -0.8660254037844345998, 0.000000000000000000, -0.5000000000000071054 ) ) ;
#2064 = CARTESIAN_POINT ( 'NONE',  ( 0.000000000000000000, 27.99999999999999645, 0.000000000000000000 ) ) ;
#2065 = PLANE ( 'NONE',  #8127 ) ;
#2066 = EDGE_CURVE ( 'NONE', #2242, #93, #4883, .T. ) ;
#2067 = VERTEX_POINT ( 'NONE', #7156 ) ;
#2068 = PRESENTATION_LAYER_ASSIGNMENT (  '', '', ( #7351 ) ) ;
#2069 = VERTEX_POINT ( 'NONE', #2271 ) ;
#2070 = VERTEX_POINT ( 'NONE', #3138 ) ;
#2071 = EDGE_CURVE ( 'NONE', #93, #8568, #614, .T. ) ;
#2072 = FACE_OUTER_BOUND ( 'NONE', #9479, .T. ) ;
#2073 = CARTESIAN_POINT ( 'NONE',  ( -3.957930336368489021E-15, -0.001000000000001000089, -19.75000000000000000 ) ) ;
#2074 = DIRECTION ( 'NONE',  ( -0.9819805060619662962, 0.000000000000000000, 0.1889822365046104902 ) ) ;
#2075 = AXIS2_PLACEMENT_3D ( 'NONE', #979, #1914, #2552 ) ;
#2076 = CARTESIAN_POINT ( 'NONE',  ( -3.355508642977407252, 19.66631150450991683, -6.145599950363634711 ) ) ;
#2077 = CARTESIAN_POINT ( 'NONE',  ( 19.75000000000000000, 25.00000000000000000, -7.291468677852036884E-14 ) ) ;
#2078 = EDGE_CURVE ( 'NONE', #5999, #5308, #6726, .T. ) ;
#2079 = AXIS2_PLACEMENT_3D ( 'NONE', #1820, #873, #4422 ) ;
#2080 = EDGE_LOOP ( 'NONE', ( #9339, #4954, #8365, #2306 ) ) ;
#2081 = AXIS2_PLACEMENT_3D ( 'NONE', #8524, #5234, #7701 ) ;
#2082 = LINE ( 'NONE', #10695, #2667 ) ;
#2083 = CARTESIAN_POINT ( 'NONE',  ( 0.2499999999999960032, 0.000000000000000000, 0.4330127018922216298 ) ) ;
#2084 = CARTESIAN_POINT ( 'NONE',  ( 2.566987298107748394, 10.00000000000000355, 5.446152422706646234 ) ) ;
#2085 = AXIS2_PLACEMENT_3D ( 'NONE', #5285, #6996, #1025 ) ;
#2086 = EDGE_CURVE ( 'NONE', #1433, #8512, #6482, .T. ) ;
#2087 = CARTESIAN_POINT ( 'NONE',  ( 15.60400172474260927, 28.00000000000000000, -12.47307621135339062 ) ) ;
#2088 = CARTESIAN_POINT ( 'NONE',  ( 12.13990010960486288, 28.00000000000000000, -10.47307621135337641 ) ) ;
#2089 = AXIS2_PLACEMENT_3D ( 'NONE', #8010, #2142, #5523 ) ;
#2090 = ORIENTED_EDGE ( 'NONE', *, *, #10525, .T. ) ;
#2091 = ORIENTED_EDGE ( 'NONE', *, *, #5927, .F. ) ;
#2092 = CARTESIAN_POINT ( 'NONE',  ( -1.500000000000000444, 83.00000000000000000, -1.500000000000000222 ) ) ;
#2093 = CARTESIAN_POINT ( 'NONE',  ( -22.78663523973255067, 5.000000000000000888, -10.19028184728269437 ) ) ;
#2094 = CARTESIAN_POINT ( 'NONE',  ( 24.62111388749999108, 1.331249999044084475, 10.19839929293507730 ) ) ;
#2095 = ORIENTED_EDGE ( 'NONE', *, *, #8426, .F. ) ;
#2096 = DIRECTION ( 'NONE',  ( 1.000000000000000000, 0.000000000000000000, 0.000000000000000000 ) ) ;
#2097 = DIRECTION ( 'NONE',  ( 0.000000000000000000, -0.000000000000000000, -1.000000000000000000 ) ) ;
#2098 = VERTEX_POINT ( 'NONE', #618 ) ;
#2099 = CARTESIAN_POINT ( 'NONE',  ( -24.62111388750000174, 3.718749999044084653, -3.015216831376932151E-15 ) ) ;
#2100 = CARTESIAN_POINT ( 'NONE',  ( 10.35533905932734733, 4.187500000000000888, -25.00000000000004263 ) ) ;
#2101 = ORIENTED_EDGE ( 'NONE', *, *, #10844, .T. ) ;
#2102 = VERTEX_POINT ( 'NONE', #9890 ) ;
#2103 = EDGE_LOOP ( 'NONE', ( #8861, #8120, #5100, #2746 ) ) ;
#2104 = AXIS2_PLACEMENT_3D ( 'NONE', #7284, #10663, #342 ) ;
#2105 = CARTESIAN_POINT ( 'NONE',  ( -24.62111388750000884, 3.781249999044084653, 10.19839929293505421 ) ) ;
#2106 = CARTESIAN_POINT ( 'NONE',  ( 24.62111388750000174, 1.456249999044084475, -10.19839929293505776 ) ) ;
#2107 = CARTESIAN_POINT ( 'NONE',  ( 10.35533905932738286, 4.812500000000000888, 24.99999999999999645 ) ) ;
#2108 = SURFACE_STYLE_FILL_AREA ( #408 ) ;
#2109 = DIRECTION ( 'NONE',  ( -0.000000000000000000, 1.000000000000000000, -0.000000000000000000 ) ) ;
#2110 = DIRECTION ( 'NONE',  ( -0.2500000000000009992, 0.8660254037844380415, 0.4330127018922199644 ) ) ;
#2111 = LINE ( 'NONE', #8959, #551 ) ;
#2112 = DIRECTION ( 'NONE',  ( -0.8660254037844380415, -0.000000000000000000, 0.5000000000000012212 ) ) ;
#2113 = VECTOR ( 'NONE', #10837, 1000.000000000000000 ) ;
#2114 = CIRCLE ( 'NONE', #2283, 7.500000000000007994 ) ;
#2115 = CARTESIAN_POINT ( 'NONE',  ( -25.00000000000000000, 2.437500000000000444, -10.35533905932738108 ) ) ;
#2116 = ORIENTED_EDGE ( 'NONE', *, *, #7733, .T. ) ;
#2117 = EDGE_LOOP ( 'NONE', ( #111, #6362 ) ) ;
#2118 = CARTESIAN_POINT ( 'NONE',  ( 0.000000000000000000, -1.026060429977008193, -22.18092213764227694 ) ) ;
#2119 = VECTOR ( 'NONE', #9055, 999.9999999999998863 ) ;
#2120 = AXIS2_PLACEMENT_3D ( 'NONE', #10162, #5971, #6093 ) ;
#2121 = CARTESIAN_POINT ( 'NONE',  ( 12.47307621135322186, 25.00000000000000000, -15.60400172474273717 ) ) ;
#2122 = ORIENTED_EDGE ( 'NONE', *, *, #9952, .F. ) ;
#2123 = CARTESIAN_POINT ( 'NONE',  ( 28.02691073765301155, 94.63433907514509258, -5.000000000000000000 ) ) ;
#2124 = CARTESIAN_POINT ( 'NONE',  ( 5.890223162633852816, 19.34316356887877930, 3.785909150703072434 ) ) ;
#2125 = FACE_OUTER_BOUND ( 'NONE', #17, .T. ) ;
#2126 = DIRECTION ( 'NONE',  ( 0.000000000000000000, -1.000000000000000000, 0.000000000000000000 ) ) ;
#2127 = AXIS2_PLACEMENT_3D ( 'NONE', #7839, #4481, #1811 ) ;
#2128 = ORIENTED_EDGE ( 'NONE', *, *, #5183, .F. ) ;
#2129 = EDGE_CURVE ( 'NONE', #9320, #9464, #4252, .T. ) ;
#2130 = VERTEX_POINT ( 'NONE', #4835 ) ;
#2131 = ORIENTED_EDGE ( 'NONE', *, *, #812, .F. ) ;
#2132 = EDGE_CURVE ( 'NONE', #3067, #8979, #1389, .T. ) ;
#2133 = DIRECTION ( 'NONE',  ( -0.000000000000000000, -1.000000000000000000, -0.000000000000000000 ) ) ;
#2134 = DIRECTION ( 'NONE',  ( 0.000000000000000000, -1.000000000000000000, 0.000000000000000000 ) ) ;
#2135 = FACE_OUTER_BOUND ( 'NONE', #5942, .T. ) ;
#2136 = LINE ( 'NONE', #8928, #8880 ) ;
#2137 = DIRECTION ( 'NONE',  ( 0.7071067811865519026, -0.3535533905932723431, 0.6123724356957903625 ) ) ;
#2138 = EDGE_CURVE ( 'NONE', #2551, #2855, #512, .T. ) ;
#2139 = VERTEX_POINT ( 'NONE', #3786 ) ;
#2140 = VECTOR ( 'NONE', #6811, 1000.000000000000114 ) ;
#2141 = EDGE_CURVE ( 'NONE', #8924, #4397, #3522, .T. ) ;
#2142 = DIRECTION ( 'NONE',  ( -1.000000000000000000, 0.000000000000000000, 0.000000000000000000 ) ) ;
#2143 = DIRECTION ( 'NONE',  ( -0.000000000000000000, -1.000000000000000000, -0.000000000000000000 ) ) ;
#2144 = DIRECTION ( 'NONE',  ( 0.000000000000000000, -1.000000000000000000, 0.000000000000000000 ) ) ;
#2145 = CARTESIAN_POINT ( 'NONE',  ( 24.62111388749999108, 3.331249999044084920, 10.19839929293507730 ) ) ;
#2146 = ORIENTED_EDGE ( 'NONE', *, *, #6976, .F. ) ;
#2147 = AXIS2_PLACEMENT_3D ( 'NONE', #10891, #3469, #6860 ) ;
#2148 = LINE ( 'NONE', #8679, #6194 ) ;
#2149 = CARTESIAN_POINT ( 'NONE',  ( 6.982120021884469452, 19.03096903053430466, -0.4999999999999756306 ) ) ;
#2150 = CARTESIAN_POINT ( 'NONE',  ( -24.62111388750000174, 2.656249999044085097, -10.19839929293506131 ) ) ;
#2151 = VECTOR ( 'NONE', #8985, 1000.000000000000114 ) ;
#2152 = ORIENTED_EDGE ( 'NONE', *, *, #7594, .T. ) ;
#2153 = EDGE_LOOP ( 'NONE', ( #9436, #3932, #7844, #3822 ) ) ;
#2154 = AXIS2_PLACEMENT_3D ( 'NONE', #10922, #10869, #3384 ) ;
#2155 = ORIENTED_EDGE ( 'NONE', *, *, #2390, .F. ) ;
#2156 = APPLICATION_CONTEXT ( 'automotive_design' ) ;
#2157 = AXIS2_PLACEMENT_3D ( 'NONE', #9612, #3803, #9558 ) ;
#2158 = DIRECTION ( 'NONE',  ( 1.000000000000000000, 0.000000000000000000, 0.000000000000000000 ) ) ;
#2159 = CARTESIAN_POINT ( 'NONE',  ( -10.19839929293507552, 3.906249999044085097, 24.62111388749999463 ) ) ;
#2160 = VECTOR ( 'NONE', #7045, 1000.000000000000000 ) ;
#2161 = CARTESIAN_POINT ( 'NONE',  ( 24.62111388750000174, 2.456249999044084475, -10.19839929293505776 ) ) ;
#2162 = CARTESIAN_POINT ( 'NONE',  ( 24.99999999999999289, 2.937500000000000444, 10.35533905932739529 ) ) ;
#2163 = PRESENTATION_STYLE_ASSIGNMENT (( #8956 ) ) ;
#2164 =( BOUNDED_CURVE ( )  B_SPLINE_CURVE ( 2, ( #9323, #5151, #8500, #5215, #8558, #1005, #5423, #284, #10497 ),
 .UNSPECIFIED., .F., .F. ) 
 B_SPLINE_CURVE_WITH_KNOTS ( ( 3, 2, 2, 2, 3 ),
 ( 0.5500000000000000444, 0.5749999999999999556, 0.5999999999999999778, 0.6250000000000000000, 0.6500000000000000222 ),
 .UNSPECIFIED. ) 
 CURVE ( )  GEOMETRIC_REPRESENTATION_ITEM ( )  RATIONAL_B_SPLINE_CURVE ( ( 1.000000000000000000, 0.9238795325112867385, 1.000000000000000000, 0.9238795325112867385, 1.000000000000000000, 0.9238795325112867385, 1.000000000000000000, 0.9238795325112867385, 1.000000000000000000 ) ) 
 REPRESENTATION_ITEM ( '' )  );
#2165 = DIRECTION ( 'NONE',  ( 0.000000000000000000, 1.000000000000000000, 0.000000000000000000 ) ) ;
#2166 = CARTESIAN_POINT ( 'NONE',  ( 25.00000000000000000, 1.612499998088169351, 0.000000000000000000 ) ) ;
#2167 = CARTESIAN_POINT ( 'NONE',  ( 2.500000000000000444, -1.000000000000003331, 0.5773502691896272854 ) ) ;
#2168 = AXIS2_PLACEMENT_3D ( 'NONE', #3642, #8826, #10385 ) ;
#2169 = CARTESIAN_POINT ( 'NONE',  ( 1.530808498934191521E-15, 1.250000000000000000, -25.00000000000000000 ) ) ;
#2170 = CARTESIAN_POINT ( 'NONE',  ( 17.67766952966369232, 2.125000000000000000, -17.67766952966369232 ) ) ;
#2171 = AXIS2_PLACEMENT_3D ( 'NONE', #10827, #10710, #7441 ) ;
#2172 = EDGE_LOOP ( 'NONE', ( #8948, #4762, #2758, #10112 ) ) ;
#2173 = ORIENTED_EDGE ( 'NONE', *, *, #4841, .T. ) ;
#2174 = EDGE_LOOP ( 'NONE', ( #9350, #7352, #1357, #4979 ) ) ;
#2175 = VECTOR ( 'NONE', #5832, 1000.000000000000000 ) ;
#2176 = DIRECTION ( 'NONE',  ( -0.8660254037844433705, 0.000000000000000000, -0.4999999999999916733 ) ) ;
#2177 = AXIS2_PLACEMENT_3D ( 'NONE', #56, #9267, #1709 ) ;
#2178 = CARTESIAN_POINT ( 'NONE',  ( 0.000000000000000000, 0.000000000000000000, 0.000000000000000000 ) ) ;
#2179 = CARTESIAN_POINT ( 'NONE',  ( 3.499999999999963141, 20.00000000000000355, 6.062177826491089050 ) ) ;
#2180 = VECTOR ( 'NONE', #1880, 1000.000000000000114 ) ;
#2181 = CARTESIAN_POINT ( 'NONE',  ( -7.875000000000116351, 28.00000000000000000, -13.63990010960484334 ) ) ;
#2182 = ORIENTED_EDGE ( 'NONE', *, *, #4781, .T. ) ;
#2183 = CARTESIAN_POINT ( 'NONE',  ( -1.399999999999998579, 0.000000000000000000, 0.000000000000000000 ) ) ;
#2184 = PLANE ( 'NONE',  #9899 ) ;
#2185 = CARTESIAN_POINT ( 'NONE',  ( 1.500000000000000000, 83.00000000000000000, 1.500000000000000000 ) ) ;
#2186 = CARTESIAN_POINT ( 'NONE',  ( -25.00000000000000000, 3.437500000000000000, -10.35533905932738108 ) ) ;
#2187 = AXIS2_PLACEMENT_3D ( 'NONE', #7889, #1040, #3735 ) ;
#2188 = ORIENTED_EDGE ( 'NONE', *, *, #10095, .T. ) ;
#2189 = EDGE_LOOP ( 'NONE', ( #6832, #8164, #8900, #9375, #8341 ) ) ;
#2190 = CARTESIAN_POINT ( 'NONE',  ( 0.000000000000000000, 88.00000000000001421, 0.000000000000000000 ) ) ;
#2191 = ADVANCED_FACE ( 'NONE', ( #3038 ), #4775, .F. ) ;
#2192 = DIRECTION ( 'NONE',  ( 0.000000000000000000, 0.000000000000000000, -1.000000000000000000 ) ) ;
#2193 = CARTESIAN_POINT ( 'NONE',  ( -4.592425496802574367E-15, 4.362499998088169129, 25.00000000000000000 ) ) ;
#2194 = CARTESIAN_POINT ( 'NONE',  ( 7.171633369868314567, 7.781088913245556071, -11.42163336986829236 ) ) ;
#2195 = CARTESIAN_POINT ( 'NONE',  ( -10.81217782649114589, 10.00000000000000355, 5.665063509461009339 ) ) ;
#2196 = EDGE_CURVE ( 'NONE', #6472, #7410, #6285, .T. ) ;
#2197 = ORIENTED_EDGE ( 'NONE', *, *, #6530, .T. ) ;
#2198 = CARTESIAN_POINT ( 'NONE',  ( 0.000000000000000000, 1.000000000000002220, -0.5773502691896270633 ) ) ;
#2199 = CARTESIAN_POINT ( 'NONE',  ( -24.62111388750000884, 3.956249999044084475, 10.19839929293505421 ) ) ;
#2200 = VERTEX_POINT ( 'NONE', #7249 ) ;
#2201 = EDGE_CURVE ( 'NONE', #859, #2, #10622, .T. ) ;
#2202 = DIRECTION ( 'NONE',  ( 0.000000000000000000, 0.000000000000000000, 1.000000000000000000 ) ) ;
#2203 =( NAMED_UNIT ( * ) SI_UNIT ( $, .STERADIAN. ) SOLID_ANGLE_UNIT ( ) );
#2204 = DIRECTION ( 'NONE',  ( -1.000000000000000000, 0.000000000000000000, 0.000000000000000000 ) ) ;
#2205 = ORIENTED_EDGE ( 'NONE', *, *, #4118, .F. ) ;
#2206 = CARTESIAN_POINT ( 'NONE',  ( -4.522825247065398226E-15, 1.968749999044084653, 24.62111388750000174 ) ) ;
#2207 = LINE ( 'NONE', #3021, #1037 ) ;
#2208 = VERTEX_POINT ( 'NONE', #8230 ) ;
#2209 = ADVANCED_FACE ( 'NONE', ( #2429 ), #5811, .F. ) ;
#2210 = ORIENTED_EDGE ( 'NONE', *, *, #10577, .F. ) ;
#2211 = CARTESIAN_POINT ( 'NONE',  ( 25.00000000000000000, 4.674999998088169129, -10.35533905932737753 ) ) ;
#2212 = DIRECTION ( 'NONE',  ( 0.000000000000000000, -2.775557561562888270E-17, -1.000000000000000000 ) ) ;
#2213 = CARTESIAN_POINT ( 'NONE',  ( -10.19839929293507552, 3.081249999044084475, 24.62111388749999463 ) ) ;
#2214 = CARTESIAN_POINT ( 'NONE',  ( -10.35533905932737575, 4.312500000000000888, -25.00000000000000000 ) ) ;
#2215 = DIRECTION ( 'NONE',  ( 0.000000000000000000, 0.000000000000000000, 1.000000000000000000 ) ) ;
#2216 = CARTESIAN_POINT ( 'NONE',  ( -25.00000000000001421, 1.174999998088169351, 10.35533905932737397 ) ) ;
#2217 = DIRECTION ( 'NONE',  ( -0.8660254037844415942, 0.000000000000000000, 0.4999999999999949485 ) ) ;
#2218 = DIRECTION ( 'NONE',  ( -0.000000000000000000, -1.000000000000000000, -0.000000000000000000 ) ) ;
#2219 = EDGE_CURVE ( 'NONE', #8585, #7956, #9533, .T. ) ;
#2220 = ORIENTED_EDGE ( 'NONE', *, *, #9236, .T. ) ;
#2221 = ORIENTED_EDGE ( 'NONE', *, *, #7234, .T. ) ;
#2222 = ORIENTED_EDGE ( 'NONE', *, *, #396, .T. ) ;
#2223 = CARTESIAN_POINT ( 'NONE',  ( 82.32050807568876394, 102.2820323027551410, 3.379762621896238883 ) ) ;
#2224 =( BOUNDED_CURVE ( )  B_SPLINE_CURVE ( 2, ( #8763, #1201, #2610, #6005, #9365, #1805, #1306, #4103, #10632 ),
 .UNSPECIFIED., .F., .F. ) 
 B_SPLINE_CURVE_WITH_KNOTS ( ( 3, 2, 2, 2, 3 ),
 ( 0.6500000000000000222, 0.6750000000000000444, 0.6999999999999999556, 0.7249999999999999778, 0.7500000000000000000 ),
 .UNSPECIFIED. ) 
 CURVE ( )  GEOMETRIC_REPRESENTATION_ITEM ( )  RATIONAL_B_SPLINE_CURVE ( ( 1.000000000000000000, 0.9238795325112867385, 1.000000000000000000, 0.9238795325112867385, 1.000000000000000000, 0.9238795325112867385, 1.000000000000000000, 0.9238795325112867385, 1.000000000000000000 ) ) 
 REPRESENTATION_ITEM ( '' )  );
#2225 = CARTESIAN_POINT ( 'NONE',  ( 0.000000000000000000, 88.00000000000001421, -4.999999999999997335 ) ) ;
#2226 = DIRECTION ( 'NONE',  ( -1.000000000000000000, -2.775557561562888984E-15, 0.000000000000000000 ) ) ;
#2227 = ORIENTED_EDGE ( 'NONE', *, *, #4533, .T. ) ;
#2228 = FACE_OUTER_BOUND ( 'NONE', #6950, .T. ) ;
#2229 = CARTESIAN_POINT ( 'NONE',  ( -15.13990010960484867, -0.001000000000001000089, 5.276923788646865177 ) ) ;
#2230 = DIRECTION ( 'NONE',  ( -0.000000000000000000, 1.000000000000000000, -0.000000000000000000 ) ) ;
#2231 = CARTESIAN_POINT ( 'NONE',  ( 9.875000000000023093, 25.00000000000000000, 20.10400172474264835 ) ) ;
#2232 = ORIENTED_EDGE ( 'NONE', *, *, #6187, .T. ) ;
#2233 = EDGE_LOOP ( 'NONE', ( #6255, #760, #10474, #8058, #10141, #1312 ) ) ;
#2234 = DIRECTION ( 'NONE',  ( 0.000000000000000000, 1.000000000000000000, -1.502202555303642096E-16 ) ) ;
#2235 = CARTESIAN_POINT ( 'NONE',  ( -15.60400172474278158, -0.001000000000001000089, -12.47307621135316680 ) ) ;
#2236 = CARTESIAN_POINT ( 'NONE',  ( 17.67766952966369232, 4.737499998088169129, -17.67766952966369232 ) ) ;
#2237 = DIRECTION ( 'NONE',  ( 0.000000000000000000, 0.000000000000000000, -1.000000000000000000 ) ) ;
#2238 = CARTESIAN_POINT ( 'NONE',  ( 3.066987298107787030, 10.00000000000000355, -6.312177826491064181 ) ) ;
#2239 = VECTOR ( 'NONE', #86, 1000.000000000000000 ) ;
#2240 = ORIENTED_EDGE ( 'NONE', *, *, #3251, .T. ) ;
#2241 = EDGE_CURVE ( 'NONE', #5566, #8414, #4050, .T. ) ;
#2242 = VERTEX_POINT ( 'NONE', #2583 ) ;
#2243 =( NAMED_UNIT ( * ) PLANE_ANGLE_UNIT ( ) SI_UNIT ( $, .RADIAN. ) );
#2244 = MECHANICAL_DESIGN_GEOMETRIC_PRESENTATION_REPRESENTATION (  '', ( #1029 ), #6496 ) ;
#2245 = SURFACE_STYLE_FILL_AREA ( #9813 ) ;
#2246 = CARTESIAN_POINT ( 'NONE',  ( -4.522825247065398226E-15, 5.143749999044084475, 24.62111388750000174 ) ) ;
#2247 = ORIENTED_EDGE ( 'NONE', *, *, #4315, .T. ) ;
#2248 = PLANE ( 'NONE',  #363 ) ;
#2249 = DIRECTION ( 'NONE',  ( 1.000000000000000000, 0.000000000000000000, 0.000000000000000000 ) ) ;
#2250 = EDGE_CURVE ( 'NONE', #5382, #57, #3190, .T. ) ;
#2251 = CARTESIAN_POINT ( 'NONE',  ( 6.999999999999998224, 19.66631150450992038, -0.1668442477450155503 ) ) ;
#2252 = VERTEX_POINT ( 'NONE', #6758 ) ;
#2253 = VECTOR ( 'NONE', #8853, 1000.000000000000000 ) ;
#2254 = DIRECTION ( 'NONE',  ( 0.000000000000000000, 1.000000000000000000, -0.000000000000000000 ) ) ;
#2255 = CARTESIAN_POINT ( 'NONE',  ( 17.40975659021752975, 3.343749999044085097, -17.40975659021752975 ) ) ;
#2256 = ORIENTED_EDGE ( 'NONE', *, *, #727, .T. ) ;
#2257 = ORIENTED_EDGE ( 'NONE', *, *, #4852, .T. ) ;
#2258 = EDGE_CURVE ( 'NONE', #6215, #1976, #839, .T. ) ;
#2259 = ADVANCED_FACE ( 'NONE', ( #9274 ), #897, .T. ) ;
#2260 = ORIENTED_EDGE ( 'NONE', *, *, #318, .F. ) ;
#2261 = ADVANCED_FACE ( 'NONE', ( #8449 ), #10119, .F. ) ;
#2262 = CARTESIAN_POINT ( 'NONE',  ( -17.67766952966368876, 4.987499998088170017, -17.67766952966369232 ) ) ;
#2263 = DIRECTION ( 'NONE',  ( -0.4999999999999947820, 0.000000000000000000, 0.8660254037844417052 ) ) ;
#2264 = CARTESIAN_POINT ( 'NONE',  ( 24.62111388750000174, 2.218749999044084653, 0.000000000000000000 ) ) ;
#2265 = ORIENTED_EDGE ( 'NONE', *, *, #7955, .T. ) ;
#2266 = CARTESIAN_POINT ( 'NONE',  ( -5.796693311223863887, 19.03096903053432598, -3.924072712834521415 ) ) ;
#2267 = EDGE_CURVE ( 'NONE', #956, #2130, #6702, .T. ) ;
#2268 = CARTESIAN_POINT ( 'NONE',  ( -1.500000000000000444, 88.00000000000001421, -1.500000000000000222 ) ) ;
#2269 = CARTESIAN_POINT ( 'NONE',  ( -11.06217782649100911, 10.00000000000000533, -6.386751345948263214 ) ) ;
#2270 = CARTESIAN_POINT ( 'NONE',  ( -10.00000000000000000, 90.00000000000001421, 5.000000000000000000 ) ) ;
#2271 = CARTESIAN_POINT ( 'NONE',  ( 24.62111388750000174, 0.2187499990440845699, 0.000000000000000000 ) ) ;
#2272 = DIRECTION ( 'NONE',  ( -0.000000000000000000, -1.000000000000000000, -0.000000000000000000 ) ) ;
#2273 = EDGE_LOOP ( 'NONE', ( #10863, #5875, #10499, #2559 ) ) ;
#2274 = EDGE_CURVE ( 'NONE', #5054, #5784, #9331, .T. ) ;
#2275 = ORIENTED_EDGE ( 'NONE', *, *, #8022, .F. ) ;
#2276 = ORIENTED_EDGE ( 'NONE', *, *, #8540, .T. ) ;
#2277 = ORIENTED_EDGE ( 'NONE', *, *, #4796, .F. ) ;
#2278 = UNCERTAINTY_MEASURE_WITH_UNIT (LENGTH_MEASURE( 1.000000000000000082E-05 ), #6262, 'distance_accuracy_value', 'NONE');
#2279 = CARTESIAN_POINT ( 'NONE',  ( -2.566987298107710203, 10.00000000000000355, -5.446152422706663998 ) ) ;
#2280 = CARTESIAN_POINT ( 'NONE',  ( 3.924072712834419718, 19.03096903053430466, 5.796693311223933165 ) ) ;
#2281 = EDGE_CURVE ( 'NONE', #4561, #4862, #2379, .T. ) ;
#2282 = AXIS2_PLACEMENT_3D ( 'NONE', #6034, #8445, #1711 ) ;
#2283 = AXIS2_PLACEMENT_3D ( 'NONE', #6812, #789, #8395 ) ;
#2284 = ORIENTED_EDGE ( 'NONE', *, *, #307, .T. ) ;
#2285 = CARTESIAN_POINT ( 'NONE',  ( 25.00000000000000000, 5.000000000000000000, 0.000000000000000000 ) ) ;
#2286 = DIRECTION ( 'NONE',  ( -0.4999999999999947820, 0.000000000000000000, 0.8660254037844417052 ) ) ;
#2287 = CARTESIAN_POINT ( 'NONE',  ( -24.62111388750000174, 2.718749999044084653, -3.015216831376932151E-15 ) ) ;
#2288 = CARTESIAN_POINT ( 'NONE',  ( 2.500000000000000444, -4.336808689942017736E-16, 1.154700538379254571 ) ) ;
#2289 = VERTEX_POINT ( 'NONE', #4207 ) ;
#2290 = VECTOR ( 'NONE', #5847, 1000.000000000000000 ) ;
#2291 = VECTOR ( 'NONE', #8076, 1000.000000000000000 ) ;
#2292 = VERTEX_POINT ( 'NONE', #8349 ) ;
#2293 = FACE_OUTER_BOUND ( 'NONE', #8366, .T. ) ;
#2294 = DIRECTION ( 'NONE',  ( -0.000000000000000000, 1.000000000000000000, -0.000000000000000000 ) ) ;
#2295 = LINE ( 'NONE', #3105, #6783 ) ;
#2296 = CIRCLE ( 'NONE', #9548, 5.000000000000000000 ) ;
#2297 = TOROIDAL_SURFACE ( 'NONE', #373, 7.399999999999999467, 0.1000000000000000472 ) ;
#2298 = CARTESIAN_POINT ( 'NONE',  ( 25.00000000000000000, -2.710505431213761085E-17, 0.000000000000000000 ) ) ;
#2299 = CARTESIAN_POINT ( 'NONE',  ( 0.5000000000000000000, 10.00000000000000355, 12.19615242270663735 ) ) ;
#2300 = ORIENTED_EDGE ( 'NONE', *, *, #3755, .T. ) ;
#2301 = ORIENTED_EDGE ( 'NONE', *, *, #2735, .T. ) ;
#2302 = VECTOR ( 'NONE', #8664, 1000.000000000000227 ) ;
#2303 = DIRECTION ( 'NONE',  ( 0.000000000000000000, -0.000000000000000000, 1.000000000000000000 ) ) ;
#2304 = CARTESIAN_POINT ( 'NONE',  ( 0.5000000000000000000, 7.781088913245555183, 13.47724133595216500 ) ) ;
#2305 = CARTESIAN_POINT ( 'NONE',  ( 24.62111388749999108, 2.331249999044084475, 10.19839929293507730 ) ) ;
#2306 = ORIENTED_EDGE ( 'NONE', *, *, #1253, .F. ) ;
#2307 = CARTESIAN_POINT ( 'NONE',  ( -4.592425496802574367E-15, 3.362499998088169129, 25.00000000000000000 ) ) ;
#2308 = LINE ( 'NONE', #3173, #8174 ) ;
#2309 = CARTESIAN_POINT ( 'NONE',  ( -9.874999999999777955, 25.00000000000000000, 17.10400172474279401 ) ) ;
#2310 = DIRECTION ( 'NONE',  ( -0.000000000000000000, -1.000000000000000000, -0.000000000000000000 ) ) ;
#2311 = ORIENTED_EDGE ( 'NONE', *, *, #4227, .F. ) ;
#2312 = ORIENTED_EDGE ( 'NONE', *, *, #1390, .T. ) ;
#2313 = AXIS2_PLACEMENT_3D ( 'NONE', #302, #9475, #4574 ) ;
#2314 = ORIENTED_EDGE ( 'NONE', *, *, #10753, .F. ) ;
#2315 = CARTESIAN_POINT ( 'NONE',  ( 1.507608415688466075E-15, 0.6437499990440845865, -24.62111388750000174 ) ) ;
#2316 = DIRECTION ( 'NONE',  ( 0.000000000000000000, -1.000000000000000000, 0.000000000000000000 ) ) ;
#2317 = CARTESIAN_POINT ( 'NONE',  ( -17.40975659021752975, 1.593749999044084431, -17.40975659021752975 ) ) ;
#2318 = ORIENTED_EDGE ( 'NONE', *, *, #3700, .F. ) ;
#2319 = CARTESIAN_POINT ( 'NONE',  ( 0.5000000000000000000, 19.03096903053429756, -6.982120021884467675 ) ) ;
#2320 = FILL_AREA_STYLE_COLOUR ( '', #1554 ) ;
#2321 = EDGE_CURVE ( 'NONE', #5377, #9220, #9117, .T. ) ;
#2322 = DIRECTION ( 'NONE',  ( -1.000000000000000000, 0.000000000000000000, 3.708321773340234242E-15 ) ) ;
#2323 = CARTESIAN_POINT ( 'NONE',  ( 5.276923788646705304, -0.001000000000001000089, 15.13990010960490196 ) ) ;
#2324 = CARTESIAN_POINT ( 'NONE',  ( -6.386751345947996761, 10.00000000000000533, -11.06217782649116366 ) ) ;
#2325 = CARTESIAN_POINT ( 'NONE',  ( -0.2500000000000019984, 0.000000000000000000, 0.4330127018922181326 ) ) ;
#2326 = CIRCLE ( 'NONE', #932, 10.50000000000000000 ) ;
#2327 = VERTEX_POINT ( 'NONE', #7570 ) ;
#2328 = ORIENTED_EDGE ( 'NONE', *, *, #2747, .F. ) ;
#2329 = AXIS2_PLACEMENT_3D ( 'NONE', #6961, #9486, #10319 ) ;
#2330 = ADVANCED_FACE ( 'NONE', ( #2534 ), #63, .T. ) ;
#2331 = AXIS2_PLACEMENT_3D ( 'NONE', #4299, #6011, #7718 ) ;
#2332 = ORIENTED_EDGE ( 'NONE', *, *, #3800, .T. ) ;
#2333 = VECTOR ( 'NONE', #1917, 1000.000000000000000 ) ;
#2334 = CARTESIAN_POINT ( 'NONE',  ( 10.19839929293506486, 1.031249999044084653, 24.62111388749999819 ) ) ;
#2335 = CIRCLE ( 'NONE', #6067, 5.100000000000006750 ) ;
#2336 = EDGE_CURVE ( 'NONE', #7939, #3078, #10843, .T. ) ;
#2337 = CARTESIAN_POINT ( 'NONE',  ( 0.000000000000000000, 5.919319018694160373E-16, -6.250000000000007105 ) ) ;
#2338 = CARTESIAN_POINT ( 'NONE',  ( 0.1668442477450440553, 19.66631150450991328, 6.999999999999995559 ) ) ;
#2339 = AXIS2_PLACEMENT_3D ( 'NONE', #687, #5824, #5766 ) ;
#2340 = CARTESIAN_POINT ( 'NONE',  ( -10.19839929293505776, 2.531249999044085097, -24.62111388750000174 ) ) ;
#2341 = CARTESIAN_POINT ( 'NONE',  ( -4.592425496802574367E-15, 3.362499998088169129, 25.00000000000000000 ) ) ;
#2342 = VERTEX_POINT ( 'NONE', #10170 ) ;
#2343 = EDGE_CURVE ( 'NONE', #9464, #9320, #2114, .T. ) ;
#2344 = ORIENTED_EDGE ( 'NONE', *, *, #8352, .F. ) ;
#2345 = VECTOR ( 'NONE', #7624, 1000.000000000000000 ) ;
#2346 = VECTOR ( 'NONE', #7492, 1000.000000000000114 ) ;
#2347 = EDGE_CURVE ( 'NONE', #6423, #4034, #2479, .T. ) ;
#2348 = ORIENTED_EDGE ( 'NONE', *, *, #810, .F. ) ;
#2349 = ORIENTED_EDGE ( 'NONE', *, *, #3770, .T. ) ;
#2350 = CARTESIAN_POINT ( 'NONE',  ( -18.60400172474257730, -0.001000000000001000089, 7.276923788646904256 ) ) ;
#2351 = AXIS2_PLACEMENT_3D ( 'NONE', #8822, #2042, #6348 ) ;
#2352 = CARTESIAN_POINT ( 'NONE',  ( -12.13990010960478827, -0.001000000000001000089, 10.47307621135345990 ) ) ;
#2353 = DIRECTION ( 'NONE',  ( 0.4999999999999917288, 0.000000000000000000, -0.8660254037844434816 ) ) ;
#2354 = FACE_OUTER_BOUND ( 'NONE', #2117, .T. ) ;
#2355 = DIRECTION ( 'NONE',  ( 0.000000000000000000, -2.775557561562888270E-17, -1.000000000000000000 ) ) ;
#2356 = VECTOR ( 'NONE', #4747, 1000.000000000000000 ) ;
#2357 = EDGE_CURVE ( 'NONE', #2862, #5242, #7519, .T. ) ;
#2358 = ORIENTED_EDGE ( 'NONE', *, *, #7732, .F. ) ;
#2359 = SURFACE_STYLE_USAGE ( .BOTH. , #1526 ) ;
#2360 = LINE ( 'NONE', #9096, #3479 ) ;
#2361 = CARTESIAN_POINT ( 'NONE',  ( -10.19839929293505776, 4.706249999044084475, -24.62111388750000174 ) ) ;
#2362 = ORIENTED_EDGE ( 'NONE', *, *, #8396, .F. ) ;
#2363 = LINE ( 'NONE', #1530, #6371 ) ;
#2364 = DIRECTION ( 'NONE',  ( 0.7803774169840349550, 0.000000000000000000, 0.6253087933663863396 ) ) ;
#2365 = FACE_OUTER_BOUND ( 'NONE', #270, .T. ) ;
#2366 = LINE ( 'NONE', #709, #10099 ) ;
#2367 = CARTESIAN_POINT ( 'NONE',  ( 24.62111388750000174, 2.281249999044085541, -10.19839929293505776 ) ) ;
#2368 = ORIENTED_EDGE ( 'NONE', *, *, #9748, .T. ) ;
#2369 = EDGE_LOOP ( 'NONE', ( #10597, #3470, #2844, #1318, #1488, #8708 ) ) ;
#2370 = EDGE_LOOP ( 'NONE', ( #7120, #9792, #2415, #10886, #8188, #8605 ) ) ;
#2371 = CARTESIAN_POINT ( 'NONE',  ( 24.99999999999999289, 5.549999998088169129, 10.35533905932739529 ) ) ;
#2372 = CARTESIAN_POINT ( 'NONE',  ( 1.399999999999998579, 0.000000000000000000, 0.000000000000000000 ) ) ;
#2373 = CARTESIAN_POINT ( 'NONE',  ( -24.62111388750000174, 0.6562499990440846531, -10.19839929293506131 ) ) ;
#2374 = ORIENTED_EDGE ( 'NONE', *, *, #2357, .T. ) ;
#2375 = DIRECTION ( 'NONE',  ( 0.000000000000000000, 0.000000000000000000, 1.000000000000000000 ) ) ;
#2376 = CARTESIAN_POINT ( 'NONE',  ( 12.13990010960486288, -0.001000000000001000089, -10.47307621135337641 ) ) ;
#2377 = CARTESIAN_POINT ( 'NONE',  ( -1.500000000000001332, 8.637664692995941434E-16, 5.750000000000000000 ) ) ;
#2378 = CARTESIAN_POINT ( 'NONE',  ( 0.000000000000000000, 31.00000000000000000, 0.000000000000000000 ) ) ;
#2379 = LINE ( 'NONE', #9172, #6360 ) ;
#2380 = VERTEX_POINT ( 'NONE', #7463 ) ;
#2381 = ORIENTED_EDGE ( 'NONE', *, *, #3014, .T. ) ;
#2382 = SHAPE_REPRESENTATION ( 'Central Drive Shaft', ( #7040 ), #8612 ) ;
#2383 = ORIENTED_EDGE ( 'NONE', *, *, #6366, .F. ) ;
#2384 = EDGE_CURVE ( 'NONE', #10229, #10544, #9701, .T. ) ;
#2385 = CARTESIAN_POINT ( 'NONE',  ( -4.522825247065398226E-15, 3.143749999044084475, 24.62111388750000174 ) ) ;
#2386 = CARTESIAN_POINT ( 'NONE',  ( -24.62111388750000884, 1.781249999044084431, 10.19839929293505421 ) ) ;
#2387 = CARTESIAN_POINT ( 'NONE',  ( 0.000000000000000000, 20.00000000000000355, 0.000000000000000000 ) ) ;
#2388 = DIRECTION ( 'NONE',  ( 1.000000000000000000, 0.000000000000000000, 0.000000000000000000 ) ) ;
#2389 = DIRECTION ( 'NONE',  ( 1.000000000000000000, 0.000000000000000000, 0.000000000000000000 ) ) ;
#2390 = EDGE_CURVE ( 'NONE', #8735, #9894, #669, .T. ) ;
#2391 = DIRECTION ( 'NONE',  ( 0.000000000000000000, 0.000000000000000000, -1.000000000000000000 ) ) ;
#2392 = CARTESIAN_POINT ( 'NONE',  ( -24.62111388750000884, 3.781249999044084653, 10.19839929293505421 ) ) ;
#2393 = LINE ( 'NONE', #8302, #2866 ) ;
#2394 = EDGE_LOOP ( 'NONE', ( #7239, #5641, #7553 ) ) ;
#2395 = EDGE_CURVE ( 'NONE', #375, #8941, #5120, .T. ) ;
#2396 = ORIENTED_EDGE ( 'NONE', *, *, #9822, .F. ) ;
#2397 = CARTESIAN_POINT ( 'NONE',  ( 12.77350269189627063, 10.00000000000000355, 3.295974604355932848E-14 ) ) ;
#2398 = EDGE_CURVE ( 'NONE', #1843, #6119, #8817, .T. ) ;
#2399 = CARTESIAN_POINT ( 'NONE',  ( -0.4330127018922225735, 0.000000000000000000, 0.2499999999999944766 ) ) ;
#2400 = DIRECTION ( 'NONE',  ( 0.000000000000000000, -2.775557561562888270E-17, -1.000000000000000000 ) ) ;
#2401 = CARTESIAN_POINT ( 'NONE',  ( 17.32475613793127422, 5.000000000000000000, 17.73196534595880536 ) ) ;
#2402 = ORIENTED_EDGE ( 'NONE', *, *, #250, .F. ) ;
#2403 = ORIENTED_EDGE ( 'NONE', *, *, #4857, .F. ) ;
#2404 =( NAMED_UNIT ( * ) PLANE_ANGLE_UNIT ( ) SI_UNIT ( $, .RADIAN. ) );
#2405 = DIRECTION ( 'NONE',  ( 0.000000000000000000, 1.000000000000000000, 0.000000000000000000 ) ) ;
#2406 = EDGE_CURVE ( 'NONE', #7146, #9698, #6523, .T. ) ;
#2407 = VERTEX_POINT ( 'NONE', #2377 ) ;
#2408 = CARTESIAN_POINT ( 'NONE',  ( 24.99999999999999289, 3.549999998088169573, 10.35533905932739529 ) ) ;
#2409 = SHAPE_DEFINITION_REPRESENTATION ( #7944, #7612 ) ;
#2410 = EDGE_CURVE ( 'NONE', #7146, #3515, #180, .T. ) ;
#2411 = FACE_OUTER_BOUND ( 'NONE', #2628, .T. ) ;
#2412 = AXIS2_PLACEMENT_3D ( 'NONE', #8935, #2955, #2049 ) ;
#2413 = DIRECTION ( 'NONE',  ( 0.000000000000000000, 0.000000000000000000, 1.000000000000000000 ) ) ;
#2414 = CARTESIAN_POINT ( 'NONE',  ( -10.19839929293507375, 1.906249999044084431, 24.62111388749999108 ) ) ;
#2415 = ORIENTED_EDGE ( 'NONE', *, *, #3422, .T. ) ;
#2416 = ORIENTED_EDGE ( 'NONE', *, *, #3776, .F. ) ;
#2417 = CARTESIAN_POINT ( 'NONE',  ( -25.00000000000001421, 5.174999998088170017, 10.35533905932737397 ) ) ;
#2418 = EDGE_CURVE ( 'NONE', #978, #8026, #9115, .T. ) ;
#2419 = LINE ( 'NONE', #4098, #8658 ) ;
#2420 = CIRCLE ( 'NONE', #10016, 27.91176187412963117 ) ;
#2421 = CARTESIAN_POINT ( 'NONE',  ( 10.19839929293505953, 0.4062499990440845421, -24.62111388750000174 ) ) ;
#2422 = LINE ( 'NONE', #7563, #3179 ) ;
#2423 = VERTEX_POINT ( 'NONE', #2427 ) ;
#2424 = CARTESIAN_POINT ( 'NONE',  ( 0.3335819196118703922, 19.34316356887877220, -6.994037468151971026 ) ) ;
#2425 = PRESENTATION_STYLE_ASSIGNMENT (( #9885 ) ) ;
#2426 = LINE ( 'NONE', #2376, #7361 ) ;
#2427 = CARTESIAN_POINT ( 'NONE',  ( -3.924072712834379750, 10.00000000000000355, -5.796693311223960698 ) ) ;
#2428 = LINE ( 'NONE', #5924, #3178 ) ;
#2429 = FACE_OUTER_BOUND ( 'NONE', #5241, .T. ) ;
#2430 =( GEOMETRIC_REPRESENTATION_CONTEXT ( 3 ) GLOBAL_UNCERTAINTY_ASSIGNED_CONTEXT ( ( #5929 ) ) GLOBAL_UNIT_ASSIGNED_CONTEXT ( ( #9834, #6322, #10564 ) ) REPRESENTATION_CONTEXT ( 'NONE', 'WORKASPACE' ) );
#2431 = CIRCLE ( 'NONE', #4592, 6.999999999999997335 ) ;
#2432 = ORIENTED_EDGE ( 'NONE', *, *, #2864, .F. ) ;
#2433 = ORIENTED_EDGE ( 'NONE', *, *, #317, .F. ) ;
#2434 = CARTESIAN_POINT ( 'NONE',  ( 24.62111388749999463, 2.331249999044084031, 10.19839929293507730 ) ) ;
#2435 = CYLINDRICAL_SURFACE ( 'NONE', #8843, 4.999999999999997335 ) ;
#2436 = CARTESIAN_POINT ( 'NONE',  ( -12.69999999999998153, 0.000000000000000000, 0.000000000000000000 ) ) ;
#2437 = DIRECTION ( 'NONE',  ( 1.000000000000000000, 0.000000000000000000, 0.000000000000000000 ) ) ;
#2438 = CARTESIAN_POINT ( 'NONE',  ( 3.061616997868383043E-15, 85.00000000000000000, 25.00000000000000000 ) ) ;
#2439 = CARTESIAN_POINT ( 'NONE',  ( 1.530808498934191521E-15, 4.862499998088169129, -25.00000000000000000 ) ) ;
#2440 = PRODUCT_RELATED_PRODUCT_CATEGORY ( 'part', '', ( #8820 ) ) ;
#2441 = CARTESIAN_POINT ( 'NONE',  ( 24.62111388750000174, 1.218749999044084431, 0.000000000000000000 ) ) ;
#2442 = DIRECTION ( 'NONE',  ( 0.000000000000000000, 1.000000000000000000, 9.470910429910644418E-17 ) ) ;
#2443 = ORIENTED_EDGE ( 'NONE', *, *, #9275, .F. ) ;
#2444 = EDGE_LOOP ( 'NONE', ( #7564, #8051, #4091, #10854, #7436 ) ) ;
#2445 = ORIENTED_EDGE ( 'NONE', *, *, #8262, .F. ) ;
#2446 = VERTEX_POINT ( 'NONE', #9888 ) ;
#2447 = DIRECTION ( 'NONE',  ( -0.000000000000000000, -1.000000000000000000, -0.000000000000000000 ) ) ;
#2448 = DIRECTION ( 'NONE',  ( 0.000000000000000000, -0.000000000000000000, 1.000000000000000000 ) ) ;
#2449 = CARTESIAN_POINT ( 'NONE',  ( 0.000000000000000000, 0.000000000000000000, 0.000000000000000000 ) ) ;
#2450 = CARTESIAN_POINT ( 'NONE',  ( 24.99999999999999289, 0.9375000000000000000, 10.35533905932739529 ) ) ;
#2451 = EDGE_CURVE ( 'NONE', #4148, #1658, #724, .T. ) ;
#2452 = CARTESIAN_POINT ( 'NONE',  ( 4.895565917430008795, 5.000000000000001776, 24.12949820052922334 ) ) ;
#2453 = AXIS2_PLACEMENT_3D ( 'NONE', #6251, #6192, #10329 ) ;
#2454 = AXIS2_PLACEMENT_3D ( 'NONE', #10841, #6640, #4936 ) ;
#2455 = EDGE_CURVE ( 'NONE', #3294, #10189, #6532, .T. ) ;
#2456 = ORIENTED_EDGE ( 'NONE', *, *, #3587, .F. ) ;
#2457 = VECTOR ( 'NONE', #9370, 1000.000000000000000 ) ;
#2458 = CYLINDRICAL_SURFACE ( 'NONE', #8971, 25.00000000000000000 ) ;
#2459 = AXIS2_PLACEMENT_3D ( 'NONE', #1045, #6129, #371 ) ;
#2460 = CARTESIAN_POINT ( 'NONE',  ( 1.500000000000000000, 83.00000000000000000, 1.500000000000000000 ) ) ;
#2461 = CARTESIAN_POINT ( 'NONE',  ( -4.946152422706591167, 10.00000000000000355, -3.433012701892276475 ) ) ;
#2462 = SHAPE_DEFINITION_REPRESENTATION ( #7769, #4232 ) ;
#2463 = CARTESIAN_POINT ( 'NONE',  ( -20.63749999999999574, 0.000000000000000000, 0.000000000000000000 ) ) ;
#2464 = DIRECTION ( 'NONE',  ( 0.000000000000000000, 1.000000000000000000, 0.000000000000000000 ) ) ;
#2465 = EDGE_CURVE ( 'NONE', #7827, #3126, #5820, .T. ) ;
#2466 = CARTESIAN_POINT ( 'NONE',  ( 10.19839929293505953, 0.4062499990440845421, -24.62111388750000174 ) ) ;
#2467 = AXIS2_PLACEMENT_3D ( 'NONE', #2325, #10679, #8910 ) ;
#2468 = VERTEX_POINT ( 'NONE', #683 ) ;
#2469 = EDGE_CURVE ( 'NONE', #10189, #9894, #6826, .T. ) ;
#2470 = CARTESIAN_POINT ( 'NONE',  ( 10.19839929293505953, 4.581249999044083587, -24.62111388750000174 ) ) ;
#2471 = CARTESIAN_POINT ( 'NONE',  ( 18.60400172474263414, 25.00000000000000000, -7.276923788646775471 ) ) ;
#2472 = CARTESIAN_POINT ( 'NONE',  ( -4.522825247065398226E-15, 2.968749999044084653, 24.62111388750000174 ) ) ;
#2473 = PLANE ( 'NONE',  #389 ) ;
#2474 = ORIENTED_EDGE ( 'NONE', *, *, #591, .F. ) ;
#2475 = CYLINDRICAL_SURFACE ( 'NONE', #6895, 5.000000000000000000 ) ;
#2476 = CARTESIAN_POINT ( 'NONE',  ( 1.500000000000001332, 0.000000000000000000, 0.000000000000000000 ) ) ;
#2477 = CARTESIAN_POINT ( 'NONE',  ( 0.000000000000000000, -55.00000000000000000, 0.000000000000000000 ) ) ;
#2478 = DIRECTION ( 'NONE',  ( 0.000000000000000000, 0.000000000000000000, 1.000000000000000000 ) ) ;
#2479 = LINE ( 'NONE', #10002, #10939 ) ;
#2480 = AXIS2_PLACEMENT_3D ( 'NONE', #4339, #7703, #134 ) ;
#2481 = ORIENTED_EDGE ( 'NONE', *, *, #9857, .F. ) ;
#2482 = AXIS2_PLACEMENT_3D ( 'NONE', #10057, #10897, #9225 ) ;
#2483 = CARTESIAN_POINT ( 'NONE',  ( -24.62111388750000174, 2.831249999044084475, -10.19839929293506131 ) ) ;
#2484 = CARTESIAN_POINT ( 'NONE',  ( -24.62111388750000174, 1.656249999044084431, -10.19839929293506131 ) ) ;
#2485 = VECTOR ( 'NONE', #10339, 1000.000000000000000 ) ;
#2486 = CARTESIAN_POINT ( 'NONE',  ( -4.149081428685724049, 5.000000000000003553, 24.37508152705383679 ) ) ;
#2487 = LINE ( 'NONE', #6775, #5340 ) ;
#2488 = CARTESIAN_POINT ( 'NONE',  ( -17.40975659021752975, 3.593749999044084653, -17.40975659021752975 ) ) ;
#2489 = DIRECTION ( 'NONE',  ( -0.000000000000000000, -1.000000000000000000, -0.000000000000000000 ) ) ;
#2490 = ORIENTED_EDGE ( 'NONE', *, *, #9451, .T. ) ;
#2491 = AXIS2_PLACEMENT_3D ( 'NONE', #9489, #6292, #7894 ) ;
#2492 = ORIENTED_EDGE ( 'NONE', *, *, #5927, .T. ) ;
#2493 = ORIENTED_EDGE ( 'NONE', *, *, #6940, .F. ) ;
#2494 = ORIENTED_EDGE ( 'NONE', *, *, #8332, .F. ) ;
#2495 = AXIS2_PLACEMENT_3D ( 'NONE', #5510, #8876, #7173 ) ;
#2496 = EDGE_LOOP ( 'NONE', ( #4124, #10919, #4863, #5660 ) ) ;
#2497 = CONICAL_SURFACE ( 'NONE', #4996, 2.000000000000000000, 1.029744258676657198 ) ;
#2498 = VECTOR ( 'NONE', #6948, 1000.000000000000114 ) ;
#2499 = CARTESIAN_POINT ( 'NONE',  ( 0.000000000000000000, 20.00000000000000355, 0.000000000000000000 ) ) ;
#2500 = DIRECTION ( 'NONE',  ( -0.5000000000000073275, 0.000000000000000000, -0.8660254037844343777 ) ) ;
#2501 = CARTESIAN_POINT ( 'NONE',  ( 82.32050807568876394, 92.28203230275514102, 0.000000000000000000 ) ) ;
#2502 =( BOUNDED_CURVE ( )  B_SPLINE_CURVE ( 2, ( #1828, #3344, #5210, #8552, #6740, #10101, #1703, #329, #4497 ),
 .UNSPECIFIED., .F., .F. ) 
 B_SPLINE_CURVE_WITH_KNOTS ( ( 3, 2, 2, 2, 3 ),
 ( 0.8500000000000000888, 0.8750000000000001110, 0.9000000000000001332, 0.9250000000000001554, 0.9500000000000000666 ),
 .UNSPECIFIED. ) 
 CURVE ( )  GEOMETRIC_REPRESENTATION_ITEM ( )  RATIONAL_B_SPLINE_CURVE ( ( 0.9999999999999996669, 0.9238795325112870716, 1.000000000000000000, 0.9238795325112867385, 1.000000000000000000, 0.9238795325112867385, 1.000000000000000000, 0.9238795325112864054, 1.000000000000000444 ) ) 
 REPRESENTATION_ITEM ( '' )  );
#2503 = CARTESIAN_POINT ( 'NONE',  ( 0.000000000000000000, 88.00000000000001421, 0.000000000000000000 ) ) ;
#2504 = CARTESIAN_POINT ( 'NONE',  ( 7.644054968599810707, 5.000000000000000000, 23.44899443080850787 ) ) ;
#2505 = AXIS2_PLACEMENT_3D ( 'NONE', #4584, #2889, #6288 ) ;
#2506 = AXIS2_PLACEMENT_3D ( 'NONE', #9860, #593, #2237 ) ;
#2507 = AXIS2_PLACEMENT_3D ( 'NONE', #495, #10606, #3018 ) ;
#2508 = ORIENTED_EDGE ( 'NONE', *, *, #469, .F. ) ;
#2509 = EDGE_CURVE ( 'NONE', #1988, #2446, #10184, .T. ) ;
#2510 = DIRECTION ( 'NONE',  ( 1.000000000000000000, 0.000000000000000000, 0.000000000000000000 ) ) ;
#2511 = DIRECTION ( 'NONE',  ( 0.000000000000000000, 0.000000000000000000, 1.000000000000000000 ) ) ;
#2512 = DIRECTION ( 'NONE',  ( -0.000000000000000000, -1.000000000000000000, -0.000000000000000000 ) ) ;
#2513 = CARTESIAN_POINT ( 'NONE',  ( 6.999999999999997335, 20.00000000000000355, 2.444036937190192402E-14 ) ) ;
#2514 = EDGE_LOOP ( 'NONE', ( #5798, #10625, #2240, #2915 ) ) ;
#2515 = CARTESIAN_POINT ( 'NONE',  ( -2.999999999999999112, -0.001000000000001000089, -19.75000000000000000 ) ) ;
#2516 = DIRECTION ( 'NONE',  ( 0.000000000000000000, 1.000000000000000000, 0.000000000000000000 ) ) ;
#2517 = ORIENTED_EDGE ( 'NONE', *, *, #5576, .F. ) ;
#2518 = CIRCLE ( 'NONE', #3405, 27.91176187412963117 ) ;
#2519 = FACE_OUTER_BOUND ( 'NONE', #3141, .T. ) ;
#2520 = CARTESIAN_POINT ( 'NONE',  ( 24.62111388750000174, 5.218749999044084653, 0.000000000000000000 ) ) ;
#2521 = ADVANCED_FACE ( 'NONE', ( #3254 ), #10013, .T. ) ;
#2522 = ORIENTED_EDGE ( 'NONE', *, *, #3539, .T. ) ;
#2523 = EDGE_CURVE ( 'NONE', #1642, #8219, #1957, .T. ) ;
#2524 = CARTESIAN_POINT ( 'NONE',  ( 24.62111388750000174, 3.393749999044084475, 0.000000000000000000 ) ) ;
#2525 = DIRECTION ( 'NONE',  ( 0.000000000000000000, -2.775557561562888270E-17, -1.000000000000000000 ) ) ;
#2526 = CARTESIAN_POINT ( 'NONE',  ( 17.40975659021752975, 4.343749999044084653, -17.40975659021752975 ) ) ;
#2527 = DIRECTION ( 'NONE',  ( 0.000000000000000000, 0.8660254037844385966, 0.5000000000000001110 ) ) ;
#2528 = ORIENTED_EDGE ( 'NONE', *, *, #7210, .F. ) ;
#2529 = DIRECTION ( 'NONE',  ( 0.000000000000000000, 0.000000000000000000, 1.000000000000000000 ) ) ;
#2530 =( LENGTH_UNIT ( ) NAMED_UNIT ( * ) SI_UNIT ( .MILLI., .METRE. ) );
#2531 = CARTESIAN_POINT ( 'NONE',  ( 18.60400172474268032, 25.00000000000000000, 7.276923788646642244 ) ) ;
#2532 = DIRECTION ( 'NONE',  ( 0.000000000000000000, 1.000000000000000000, 0.000000000000000000 ) ) ;
#2533 = CYLINDRICAL_SURFACE ( 'NONE', #2482, 10.50000000000000000 ) ;
#2534 = FACE_OUTER_BOUND ( 'NONE', #2370, .T. ) ;
#2535 = EDGE_CURVE ( 'NONE', #6001, #1446, #9127, .T. ) ;
#2536 = EDGE_LOOP ( 'NONE', ( #9626, #7411, #6470, #3601 ) ) ;
#2537 = ORIENTED_EDGE ( 'NONE', *, *, #182, .T. ) ;
#2538 = CARTESIAN_POINT ( 'NONE',  ( -18.60400172474273361, -0.001000000000001000089, -7.276923788646511682 ) ) ;
#2539 = CARTESIAN_POINT ( 'NONE',  ( -17.40975659021752975, 4.768749999044085364, -17.40975659021752975 ) ) ;
#2540 = CARTESIAN_POINT ( 'NONE',  ( 10.19839929293505953, 1.581249999044084475, -24.62111388750000174 ) ) ;
#2541 = CARTESIAN_POINT ( 'NONE',  ( -17.67766952966369232, 0.6250000000000000000, 17.67766952966368876 ) ) ;
#2542 = LINE ( 'NONE', #8296, #3113 ) ;
#2543 = EDGE_CURVE ( 'NONE', #5838, #9967, #10850, .T. ) ;
#2544 = CARTESIAN_POINT ( 'NONE',  ( -25.00000000000001066, 2.174999998088168685, 10.35533905932737397 ) ) ;
#2545 = CARTESIAN_POINT ( 'NONE',  ( -6.296693311223937606, 19.03096903053434019, 3.058047309049956031 ) ) ;
#2546 = CARTESIAN_POINT ( 'NONE',  ( 25.00000000000000000, 0.06249999999999997224, -10.35533905932737753 ) ) ;
#2547 = CARTESIAN_POINT ( 'NONE',  ( -3.000000000000000888, 28.00000000000000000, -15.75000000000000355 ) ) ;
#2548 = ORIENTED_EDGE ( 'NONE', *, *, #5914, .T. ) ;
#2549 = ORIENTED_EDGE ( 'NONE', *, *, #8776, .T. ) ;
#2550 = ORIENTED_EDGE ( 'NONE', *, *, #6336, .T. ) ;
#2551 = VERTEX_POINT ( 'NONE', #9288 ) ;
#2552 = DIRECTION ( 'NONE',  ( 0.000000000000000000, -0.000000000000000000, 1.000000000000000000 ) ) ;
#2553 = CARTESIAN_POINT ( 'NONE',  ( -5.000000000000000000, 90.00000000000001421, 0.000000000000000000 ) ) ;
#2554 = CARTESIAN_POINT ( 'NONE',  ( -5.665063509461194968, 10.00000000000000355, 10.81217782649104109 ) ) ;
#2555 = DIRECTION ( 'NONE',  ( 0.000000000000000000, -1.000000000000000000, 0.000000000000000000 ) ) ;
#2556 = LINE ( 'NONE', #6179, #10059 ) ;
#2557 = CARTESIAN_POINT ( 'NONE',  ( 24.81930730699091114, 5.000000000000000000, 2.826949417608202619 ) ) ;
#2558 = ORIENTED_EDGE ( 'NONE', *, *, #812, .T. ) ;
#2559 = ORIENTED_EDGE ( 'NONE', *, *, #6320, .F. ) ;
#2560 = CARTESIAN_POINT ( 'NONE',  ( -1.399999999999998579, -2.053912595556539452E-16, -7.400000000000007461 ) ) ;
#2561 = CARTESIAN_POINT ( 'NONE',  ( 0.000000000000000000, 8.000000000000003553, 0.000000000000000000 ) ) ;
#2562 = DIRECTION ( 'NONE',  ( 0.000000000000000000, 0.000000000000000000, -1.000000000000000000 ) ) ;
#2563 = CARTESIAN_POINT ( 'NONE',  ( 0.000000000000000000, 20.00000000000000355, 6.999999999999997335 ) ) ;
#2564 =( BOUNDED_CURVE ( )  B_SPLINE_CURVE ( 2, ( #2307, #5741, #1585, #2408, #3981, #5635, #7331, #8324, #8993 ),
 .UNSPECIFIED., .F., .F. ) 
 B_SPLINE_CURVE_WITH_KNOTS ( ( 3, 2, 2, 2, 3 ),
 ( 0.5500000000000000444, 0.5749999999999999556, 0.5999999999999999778, 0.6250000000000000000, 0.6500000000000000222 ),
 .UNSPECIFIED. ) 
 CURVE ( )  GEOMETRIC_REPRESENTATION_ITEM ( )  RATIONAL_B_SPLINE_CURVE ( ( 1.000000000000000000, 0.9238795325112867385, 1.000000000000000000, 0.9238795325112867385, 1.000000000000000000, 0.9238795325112867385, 1.000000000000000000, 0.9238795325112867385, 1.000000000000000000 ) ) 
 REPRESENTATION_ITEM ( '' )  );
#2565 = ORIENTED_EDGE ( 'NONE', *, *, #9839, .F. ) ;
#2566 = DIRECTION ( 'NONE',  ( 0.000000000000000000, 0.000000000000000000, 1.000000000000000000 ) ) ;
#2567 = CONTEXT_DEPENDENT_SHAPE_REPRESENTATION ( #7887, #176 ) ;
#2568 = LINE ( 'NONE', #878, #9598 ) ;
#2569 = FACE_OUTER_BOUND ( 'NONE', #4759, .T. ) ;
#2570 = LINE ( 'NONE', #1768, #10387 ) ;
#2571 = EDGE_CURVE ( 'NONE', #2830, #6236, #911, .T. ) ;
#2572 = VERTEX_POINT ( 'NONE', #8360 ) ;
#2573 = EDGE_CURVE ( 'NONE', #5761, #5725, #801, .T. ) ;
#2574 = CARTESIAN_POINT ( 'NONE',  ( 24.62111388750000174, 3.456249999044084920, -10.19839929293505776 ) ) ;
#2575 = DIRECTION ( 'NONE',  ( 0.000000000000000000, -1.000000000000000000, 0.000000000000000000 ) ) ;
#2576 = DIRECTION ( 'NONE',  ( 0.000000000000000000, 0.000000000000000000, 1.000000000000000000 ) ) ;
#2577 = ORIENTED_EDGE ( 'NONE', *, *, #5050, .F. ) ;
#2578 = DIRECTION ( 'NONE',  ( -0.000000000000000000, -1.000000000000000000, -0.000000000000000000 ) ) ;
#2579 = CARTESIAN_POINT ( 'NONE',  ( -5.276923788646491253, -0.001000000000001000089, 15.13990010960497834 ) ) ;
#2580 = AXIS2_PLACEMENT_3D ( 'NONE', #5534, #7093, #8743 ) ;
#2581 = CARTESIAN_POINT ( 'NONE',  ( 24.99999999999999289, 1.549999998088169129, 10.35533905932739529 ) ) ;
#2582 = CARTESIAN_POINT ( 'NONE',  ( 0.000000000000000000, 10.00000000000000355, 0.000000000000000000 ) ) ;
#2583 = CARTESIAN_POINT ( 'NONE',  ( -4.592425496802574367E-15, 3.750000000000000000, 25.00000000000000000 ) ) ;
#2584 = EDGE_CURVE ( 'NONE', #10364, #9293, #7829, .T. ) ;
#2585 = EDGE_CURVE ( 'NONE', #2663, #5323, #6852, .T. ) ;
#2586 = ADVANCED_FACE ( 'NONE', ( #4950 ), #7478, .T. ) ;
#2587 = AXIS2_PLACEMENT_3D ( 'NONE', #1774, #3529, #6805 ) ;
#2588 = VERTEX_POINT ( 'NONE', #1681 ) ;
#2589 = ORIENTED_EDGE ( 'NONE', *, *, #1321, .T. ) ;
#2590 = ORIENTED_EDGE ( 'NONE', *, *, #261, .F. ) ;
#2591 = AXIS2_PLACEMENT_3D ( 'NONE', #5397, #3033, #7925 ) ;
#2592 = EDGE_CURVE ( 'NONE', #10544, #6448, #8165, .T. ) ;
#2593 = DIRECTION ( 'NONE',  ( -2.168404344971010347E-16, 0.000000000000000000, -1.000000000000000000 ) ) ;
#2594 = CARTESIAN_POINT ( 'NONE',  ( -24.62111388750000884, 2.956249999044084475, 10.19839929293505421 ) ) ;
#2595 = CARTESIAN_POINT ( 'NONE',  ( 5.510910596163089556E-16, 7.000000000000003553, 4.500000000000000888 ) ) ;
#2596 = CARTESIAN_POINT ( 'NONE',  ( 17.40975659021752975, 1.518749999044084698, -17.40975659021752975 ) ) ;
#2597 = CARTESIAN_POINT ( 'NONE',  ( -4.522825247065398226E-15, 2.968749999044084653, 24.62111388750000174 ) ) ;
#2598 = LINE ( 'NONE', #5338, #848 ) ;
#2599 = CARTESIAN_POINT ( 'NONE',  ( -3.223142256880076948E-15, -0.001000000000001000089, -12.75000000000000178 ) ) ;
#2600 = CARTESIAN_POINT ( 'NONE',  ( 7.276923788646707969, 25.00000000000000000, 18.60400172474265190 ) ) ;
#2601 = VECTOR ( 'NONE', #7327, 1000.000000000000000 ) ;
#2602 = CARTESIAN_POINT ( 'NONE',  ( 25.00000000000000000, 1.062500000000000222, -10.35533905932737753 ) ) ;
#2603 = ADVANCED_FACE ( 'NONE', ( #3667 ), #1146, .F. ) ;
#2604 = CARTESIAN_POINT ( 'NONE',  ( -9.874999999999777955, 25.00000000000000000, 17.10400172474279401 ) ) ;
#2605 = ORIENTED_EDGE ( 'NONE', *, *, #7016, .T. ) ;
#2606 = VERTEX_POINT ( 'NONE', #5235 ) ;
#2607 = ORIENTED_EDGE ( 'NONE', *, *, #10639, .F. ) ;
#2608 = LINE ( 'NONE', #5349, #5434 ) ;
#2609 = ADVANCED_FACE ( 'NONE', ( #2715, #6166 ), #7051, .F. ) ;
#2610 = CARTESIAN_POINT ( 'NONE',  ( -17.67766952966368876, 3.987499998088168685, -17.67766952966369232 ) ) ;
#2611 = VERTEX_POINT ( 'NONE', #4399 ) ;
#2612 = CARTESIAN_POINT ( 'NONE',  ( 1.500000000000001332, -1.533495552763497570E-16, -5.525000000000006573 ) ) ;
#2613 = DIRECTION ( 'NONE',  ( -0.000000000000000000, -1.000000000000000000, -0.000000000000000000 ) ) ;
#2614 = CARTESIAN_POINT ( 'NONE',  ( -0.5000000000000000000, 10.00000000000000355, 12.19615242270663202 ) ) ;
#2615 = LINE ( 'NONE', #4352, #7412 ) ;
#2616 = CARTESIAN_POINT ( 'NONE',  ( -12.92820323027551765, 10.00000000000000355, 0.1339745962154219039 ) ) ;
#2617 = VERTEX_POINT ( 'NONE', #8697 ) ;
#2618 = ORIENTED_EDGE ( 'NONE', *, *, #3422, .F. ) ;
#2619 = CARTESIAN_POINT ( 'NONE',  ( -19.75000000000003197, -0.001000000000001000089, -2.999999999999789946 ) ) ;
#2620 =( LENGTH_UNIT ( ) NAMED_UNIT ( * ) SI_UNIT ( .MILLI., .METRE. ) );
#2621 = CYLINDRICAL_SURFACE ( 'NONE', #8239, 25.00000000000000000 ) ;
#2622 = CARTESIAN_POINT ( 'NONE',  ( -3.223142256880076948E-15, 25.00000000000000000, -15.75000000000000000 ) ) ;
#2623 = DIRECTION ( 'NONE',  ( 0.000000000000000000, 0.000000000000000000, 1.000000000000000000 ) ) ;
#2624 = CIRCLE ( 'NONE', #6213, 25.00000000000000000 ) ;
#2625 = AXIS2_PLACEMENT_3D ( 'NONE', #7300, #8958, #7247 ) ;
#2626 = DIRECTION ( 'NONE',  ( 0.8660254037844362651, 0.000000000000000000, -0.5000000000000041078 ) ) ;
#2627 = CARTESIAN_POINT ( 'NONE',  ( -24.62111388750000174, 4.718749999044084653, -3.015216831376932151E-15 ) ) ;
#2628 = EDGE_LOOP ( 'NONE', ( #8081, #5108, #1233, #8278 ) ) ;
#2629 = VECTOR ( 'NONE', #9256, 1000.000000000000000 ) ;
#2630 = AXIS2_PLACEMENT_3D ( 'NONE', #4552, #2143, #336 ) ;
#2631 = CARTESIAN_POINT ( 'NONE',  ( -17.40975659021752975, 0.7687499990440846975, -17.40975659021752975 ) ) ;
#2632 = CARTESIAN_POINT ( 'NONE',  ( 24.62111388749999463, 3.331249999044084920, 10.19839929293507730 ) ) ;
#2633 = DIRECTION ( 'NONE',  ( 0.000000000000000000, 1.000000000000000000, 0.000000000000000000 ) ) ;
#2634 = PLANE ( 'NONE',  #576 ) ;
#2635 = DIRECTION ( 'NONE',  ( -0.000000000000000000, -0.000000000000000000, 1.000000000000000000 ) ) ;
#2636 = ORIENTED_EDGE ( 'NONE', *, *, #7018, .T. ) ;
#2637 = FACE_OUTER_BOUND ( 'NONE', #3754, .T. ) ;
#2638 =( LENGTH_UNIT ( ) NAMED_UNIT ( * ) SI_UNIT ( .MILLI., .METRE. ) );
#2639 = FACE_OUTER_BOUND ( 'NONE', #8178, .T. ) ;
#2640 = PLANE ( 'NONE',  #572 ) ;
#2641 = CARTESIAN_POINT ( 'NONE',  ( 10.35533905932738286, 2.424999998088169129, 24.99999999999999645 ) ) ;
#2642 = DIRECTION ( 'NONE',  ( 0.000000000000000000, 1.000000000000000000, 0.000000000000000000 ) ) ;
#2643 = CARTESIAN_POINT ( 'NONE',  ( 25.00000000000000000, 4.062500000000000000, -10.35533905932737753 ) ) ;
#2644 = ORIENTED_EDGE ( 'NONE', *, *, #7733, .F. ) ;
#2645 = DIRECTION ( 'NONE',  ( 0.000000000000000000, -2.775557561562888270E-17, -1.000000000000000000 ) ) ;
#2646 = CARTESIAN_POINT ( 'NONE',  ( 10.19839929293505953, 2.581249999044084475, -24.62111388750000174 ) ) ;
#2647 = CARTESIAN_POINT ( 'NONE',  ( -10.19839929293505776, 0.7062499990440844755, -24.62111388750000174 ) ) ;
#2648 = AXIS2_PLACEMENT_3D ( 'NONE', #6097, #2578, #4377 ) ;
#2649 = EDGE_CURVE ( 'NONE', #811, #8502, #2025, .T. ) ;
#2650 = EDGE_CURVE ( 'NONE', #2786, #9703, #10750, .T. ) ;
#2651 = CARTESIAN_POINT ( 'NONE',  ( -4.592425496802574367E-15, 4.362499998088169129, 25.00000000000000000 ) ) ;
#2652 = CARTESIAN_POINT ( 'NONE',  ( 17.40975659021752620, 5.093749999044084653, 17.40975659021753330 ) ) ;
#2653 = CARTESIAN_POINT ( 'NONE',  ( -4.592425496802574367E-15, 3.362499998088169129, 25.00000000000000000 ) ) ;
#2654 = ORIENTED_EDGE ( 'NONE', *, *, #2571, .F. ) ;
#2655 = DIRECTION ( 'NONE',  ( 2.168404344971010347E-16, -0.000000000000000000, 1.000000000000000000 ) ) ;
#2656 = FACE_BOUND ( 'NONE', #8999, .T. ) ;
#2657 = CARTESIAN_POINT ( 'NONE',  ( 8.499999999999998224, 92.59807621135333022, 5.000000000000000000 ) ) ;
#2658 = CARTESIAN_POINT ( 'NONE',  ( 10.35533905932738286, 4.812500000000000888, 24.99999999999999645 ) ) ;
#2659 = CARTESIAN_POINT ( 'NONE',  ( 1.530808498934191521E-15, 0.2500000000000000000, -25.00000000000000000 ) ) ;
#2660 = LINE ( 'NONE', #9418, #9403 ) ;
#2661 = ADVANCED_FACE ( 'NONE', ( #8754 ), #1243, .T. ) ;
#2662 = ORIENTED_EDGE ( 'NONE', *, *, #646, .F. ) ;
#2663 = VERTEX_POINT ( 'NONE', #1794 ) ;
#2664 = CIRCLE ( 'NONE', #7430, 6.999999999999997335 ) ;
#2665 = CARTESIAN_POINT ( 'NONE',  ( 10.47307621135324496, -0.001000000000001000089, -12.13990010960497479 ) ) ;
#2666 = EDGE_CURVE ( 'NONE', #8512, #4041, #2869, .T. ) ;
#2667 = VECTOR ( 'NONE', #4745, 1000.000000000000000 ) ;
#2668 = CARTESIAN_POINT ( 'NONE',  ( 0.000000000000000000, 10.00000000000000355, 0.000000000000000000 ) ) ;
#2669 = ORIENTED_EDGE ( 'NONE', *, *, #1657, .F. ) ;
#2670 = DIRECTION ( 'NONE',  ( -0.000000000000000000, -1.000000000000000000, -0.000000000000000000 ) ) ;
#2671 = PLANE ( 'NONE',  #253 ) ;
#2672 = VECTOR ( 'NONE', #5836, 1000.000000000000000 ) ;
#2673 = DIRECTION ( 'NONE',  ( -0.000000000000000000, -1.000000000000000000, -0.000000000000000000 ) ) ;
#2674 = DIRECTION ( 'NONE',  ( 1.000000000000000000, 0.000000000000000000, 3.491481338843133355E-15 ) ) ;
#2675 = DIRECTION ( 'NONE',  ( -0.7071067811865519026, -0.3535533905932723431, -0.6123724356957903625 ) ) ;
#2676 = ADVANCED_FACE ( 'NONE', ( #3609 ), #1906, .F. ) ;
#2677 = EDGE_LOOP ( 'NONE', ( #10778, #9981, #6427, #3056 ) ) ;
#2678 = VECTOR ( 'NONE', #529, 1000.000000000000000 ) ;
#2679 = AXIS2_PLACEMENT_3D ( 'NONE', #2891, #8537, #7837 ) ;
#2680 = ORIENTED_EDGE ( 'NONE', *, *, #3251, .F. ) ;
#2681 = AXIS2_PLACEMENT_3D ( 'NONE', #6108, #1901, #6877 ) ;
#2682 = LINE ( 'NONE', #9149, #3688 ) ;
#2683 = CARTESIAN_POINT ( 'NONE',  ( -18.39893213276270956, 4.993656359492002039, -16.95640692656465731 ) ) ;
#2684 = CARTESIAN_POINT ( 'NONE',  ( 3.000000000000000888, 28.00000000000000000, 15.75000000000000355 ) ) ;
#2685 = CARTESIAN_POINT ( 'NONE',  ( 1.507608415688466075E-15, 1.643749999044084475, -24.62111388750000174 ) ) ;
#2686 = VERTEX_POINT ( 'NONE', #6997 ) ;
#2687 = AXIS2_PLACEMENT_3D ( 'NONE', #10501, #8680, #1124 ) ;
#2688 = CARTESIAN_POINT ( 'NONE',  ( -6.223805082245704945, 19.34316356887878996, -3.208128317448997180 ) ) ;
#2689 = VECTOR ( 'NONE', #8361, 1000.000000000000000 ) ;
#2690 = DIRECTION ( 'NONE',  ( 0.000000000000000000, 1.000000000000000000, 0.000000000000000000 ) ) ;
#2691 = ADVANCED_FACE ( 'NONE', ( #6053, #2882, #9352, #8637, #4461, #2656, #8525, #974, #7702, #10354, #133, #9414, #3494, #6882 ), #192, .F. ) ;
#2692 = CARTESIAN_POINT ( 'NONE',  ( 0.000000000000000000, 10.00000000000000355, 0.000000000000000000 ) ) ;
#2693 = CARTESIAN_POINT ( 'NONE',  ( 7.276923788646707969, 25.00000000000000000, 18.60400172474265190 ) ) ;
#2694 = CIRCLE ( 'NONE', #10821, 2.999999999999999112 ) ;
#2695 = CARTESIAN_POINT ( 'NONE',  ( 24.62111388749999463, 1.331249999044084475, 10.19839929293507730 ) ) ;
#2696 = DIRECTION ( 'NONE',  ( 0.000000000000000000, 0.000000000000000000, -1.000000000000000000 ) ) ;
#2697 = CIRCLE ( 'NONE', #3956, 5.000000000000000000 ) ;
#2698 = CARTESIAN_POINT ( 'NONE',  ( 1.507608415688466075E-15, 4.468749999044084653, -24.62111388750000174 ) ) ;
#2699 = LINE ( 'NONE', #6981, #2485 ) ;
#2700 = VERTEX_POINT ( 'NONE', #5597 ) ;
#2701 = CARTESIAN_POINT ( 'NONE',  ( -10.35533905932737575, 0.9249999980881692396, -25.00000000000000000 ) ) ;
#2702 = CARTESIAN_POINT ( 'NONE',  ( 10.35533905932738641, 1.799999998088168685, -24.99999999999999289 ) ) ;
#2703 = FACE_BOUND ( 'NONE', #3986, .T. ) ;
#2704 = CARTESIAN_POINT ( 'NONE',  ( -17.67766952966369232, 2.237499998088169573, 17.67766952966368876 ) ) ;
#2705 = VECTOR ( 'NONE', #263, 1000.000000000000114 ) ;
#2706 = DIRECTION ( 'NONE',  ( 0.000000000000000000, 0.000000000000000000, 1.000000000000000000 ) ) ;
#2707 = CARTESIAN_POINT ( 'NONE',  ( 1.530808498934191521E-15, 3.250000000000000444, -25.00000000000000000 ) ) ;
#2708 = ORIENTED_EDGE ( 'NONE', *, *, #10525, .F. ) ;
#2709 = ORIENTED_EDGE ( 'NONE', *, *, #6287, .F. ) ;
#2710 = LINE ( 'NONE', #2538, #9138 ) ;
#2711 = CARTESIAN_POINT ( 'NONE',  ( -24.62111388750000174, 4.831249999044085364, -10.19839929293506131 ) ) ;
#2712 = CARTESIAN_POINT ( 'NONE',  ( 1.530808498934191521E-15, 0.2500000000000000000, -25.00000000000000000 ) ) ;
#2713 = CARTESIAN_POINT ( 'NONE',  ( -4.592425496802574367E-15, 2.362499998088169129, 25.00000000000000000 ) ) ;
#2714 = CARTESIAN_POINT ( 'NONE',  ( 10.19839929293505953, 3.406249999044085097, -24.62111388750000174 ) ) ;
#2715 = FACE_BOUND ( 'NONE', #400, .T. ) ;
#2716 = DIRECTION ( 'NONE',  ( 0.000000000000000000, -2.775557561562887961E-17, -1.000000000000000000 ) ) ;
#2717 = DIRECTION ( 'NONE',  ( -0.000000000000000000, -1.000000000000000000, -0.000000000000000000 ) ) ;
#2718 = CARTESIAN_POINT ( 'NONE',  ( 10.35533905932737930, 0.1874999999999999722, -25.00000000000000000 ) ) ;
#2719 = CARTESIAN_POINT ( 'NONE',  ( -4.592425496802574367E-15, 2.362499998088169129, 25.00000000000000000 ) ) ;
#2720 = ORIENTED_EDGE ( 'NONE', *, *, #8416, .T. ) ;
#2721 = EDGE_LOOP ( 'NONE', ( #9336, #6495, #7057, #3540 ) ) ;
#2722 = EDGE_CURVE ( 'NONE', #8620, #7956, #5439, .T. ) ;
#2723 = ORIENTED_EDGE ( 'NONE', *, *, #4529, .F. ) ;
#2724 = ORIENTED_EDGE ( 'NONE', *, *, #10033, .F. ) ;
#2725 = CARTESIAN_POINT ( 'NONE',  ( -6.296693311223874545, 10.00000000000000355, -3.058047309050087925 ) ) ;
#2726 = ADVANCED_FACE ( 'NONE', ( #3943 ), #9734, .T. ) ;
#2727 = LINE ( 'NONE', #6834, #7121 ) ;
#2728 = EDGE_LOOP ( 'NONE', ( #1524, #3074 ) ) ;
#2729 = DIRECTION ( 'NONE',  ( 0.000000000000000000, 0.000000000000000000, 1.000000000000000000 ) ) ;
#2730 = DIRECTION ( 'NONE',  ( 0.8660254037844397068, 0.000000000000000000, -0.4999999999999979461 ) ) ;
#2731 = CARTESIAN_POINT ( 'NONE',  ( 68.37372805638788975, 92.28203230275514102, 5.000000000000000000 ) ) ;
#2732 = LINE ( 'NONE', #2783, #6719 ) ;
#2733 = CARTESIAN_POINT ( 'NONE',  ( -17.67766952966368876, 1.375000000000000000, -17.67766952966369232 ) ) ;
#2734 = PLANE ( 'NONE',  #2459 ) ;
#2735 = EDGE_CURVE ( 'NONE', #6733, #2289, #7394, .T. ) ;
#2736 = ORIENTED_EDGE ( 'NONE', *, *, #6328, .T. ) ;
#2737 = ADVANCED_FACE ( 'NONE', ( #3830 ), #4623, .F. ) ;
#2738 = CARTESIAN_POINT ( 'NONE',  ( -4.592425496802574367E-15, 2.750000000000000000, 25.00000000000000000 ) ) ;
#2739 = FACE_OUTER_BOUND ( 'NONE', #9020, .T. ) ;
#2740 = CARTESIAN_POINT ( 'NONE',  ( -24.62111388750000174, 1.893749999044084475, -3.015216831376932151E-15 ) ) ;
#2741 = DIRECTION ( 'NONE',  ( 0.000000000000000000, 0.000000000000000000, -1.000000000000000000 ) ) ;
#2742 = ITEM_DEFINED_TRANSFORMATION ( 'NONE', 'NONE', #869,  #7040 ) ;
#2743 = LINE ( 'NONE', #7854, #2180 ) ;
#2744 = DIRECTION ( 'NONE',  ( -0.000000000000000000, 1.000000000000000000, -0.000000000000000000 ) ) ;
#2745 = CARTESIAN_POINT ( 'NONE',  ( 17.40975659021752620, 4.093749999044084653, 17.40975659021753330 ) ) ;
#2746 = ORIENTED_EDGE ( 'NONE', *, *, #1960, .F. ) ;
#2747 = EDGE_CURVE ( 'NONE', #5785, #5770, #527, .T. ) ;
#2748 = EDGE_CURVE ( 'NONE', #6448, #9593, #9636, .T. ) ;
#2749 = CARTESIAN_POINT ( 'NONE',  ( -3.058047309049932938, 10.00000000000000355, -6.296693311223948264 ) ) ;
#2750 = CARTESIAN_POINT ( 'NONE',  ( 24.62111388750000174, 4.218749999044084653, 0.000000000000000000 ) ) ;
#2751 = CARTESIAN_POINT ( 'NONE',  ( -24.62111388750000174, 0.8937499990440845865, -3.015216831376932151E-15 ) ) ;
#2752 = ORIENTED_EDGE ( 'NONE', *, *, #936, .F. ) ;
#2753 = CARTESIAN_POINT ( 'NONE',  ( -15.60400172474251868, -0.001000000000001000089, 12.47307621135349720 ) ) ;
#2754 = DIRECTION ( 'NONE',  ( -0.000000000000000000, 1.000000000000000000, -0.000000000000000000 ) ) ;
#2755 = CARTESIAN_POINT ( 'NONE',  ( -6.296693311223937606, 10.00000000000000355, 3.058047309049956031 ) ) ;
#2756 = DIRECTION ( 'NONE',  ( 0.000000000000000000, 0.000000000000000000, 1.000000000000000000 ) ) ;
#2757 = ORIENTED_EDGE ( 'NONE', *, *, #7215, .F. ) ;
#2758 = ORIENTED_EDGE ( 'NONE', *, *, #5514, .F. ) ;
#2759 = ADVANCED_FACE ( 'NONE', ( #8185 ), #9836, .F. ) ;
#2760 = CARTESIAN_POINT ( 'NONE',  ( 1.530808498934191521E-15, 2.250000000000000444, -25.00000000000000000 ) ) ;
#2761 = CARTESIAN_POINT ( 'NONE',  ( 17.40975659021752975, 2.518749999044084475, -17.40975659021752975 ) ) ;
#2762 = DIRECTION ( 'NONE',  ( 0.000000000000000000, 1.000000000000000000, 0.000000000000000000 ) ) ;
#2763 = CARTESIAN_POINT ( 'NONE',  ( -17.67766952966368876, 4.987499998088170017, -17.67766952966369232 ) ) ;
#2764 = CARTESIAN_POINT ( 'NONE',  ( 1.507608415688466075E-15, 4.468749999044084653, -24.62111388750000174 ) ) ;
#2765 = FACE_OUTER_BOUND ( 'NONE', #1497, .T. ) ;
#2766 = DIRECTION ( 'NONE',  ( 0.000000000000000000, 1.000000000000000000, 0.000000000000000000 ) ) ;
#2767 = CARTESIAN_POINT ( 'NONE',  ( 0.000000000000000000, -58.00000000000000000, 0.000000000000000000 ) ) ;
#2768 = CYLINDRICAL_SURFACE ( 'NONE', #1413, 5.000000000000000000 ) ;
#2769 = CIRCLE ( 'NONE', #2079, 2.000000000000004441 ) ;
#2770 = CARTESIAN_POINT ( 'NONE',  ( -24.62111388750000174, 4.656249999044085541, -10.19839929293506131 ) ) ;
#2771 = EDGE_LOOP ( 'NONE', ( #10171, #5911, #8645, #8745 ) ) ;
#2772 = ORIENTED_EDGE ( 'NONE', *, *, #317, .T. ) ;
#2773 = ORIENTED_EDGE ( 'NONE', *, *, #4163, .T. ) ;
#2774 = DIRECTION ( 'NONE',  ( 0.5000000000000042188, 0.000000000000000000, 0.8660254037844362651 ) ) ;
#2775 = VECTOR ( 'NONE', #7477, 1000.000000000000000 ) ;
#2776 = VECTOR ( 'NONE', #1829, 999.9999999999998863 ) ;
#2777 = PRODUCT_RELATED_PRODUCT_CATEGORY ( 'part', '', ( #6104 ) ) ;
#2778 = DIRECTION ( 'NONE',  ( 1.000000000000000000, 0.000000000000000000, 0.000000000000000000 ) ) ;
#2779 = ORIENTED_EDGE ( 'NONE', *, *, #5251, .T. ) ;
#2780 = LINE ( 'NONE', #6176, #258 ) ;
#2781 = FACE_OUTER_BOUND ( 'NONE', #2233, .T. ) ;
#2782 = CYLINDRICAL_SURFACE ( 'NONE', #5536, 10.50000000000000000 ) ;
#2783 = CARTESIAN_POINT ( 'NONE',  ( 14.00000000000000533, 2.449293598294711838E-16, -2.000000000000004441 ) ) ;
#2784 = CARTESIAN_POINT ( 'NONE',  ( 3.061616997868383043E-15, 85.00000000000000000, 25.00000000000000000 ) ) ;
#2785 = CARTESIAN_POINT ( 'NONE',  ( 1.507608415688466075E-15, 4.643749999044084475, -24.62111388750000174 ) ) ;
#2786 = VERTEX_POINT ( 'NONE', #10518 ) ;
#2787 = VERTEX_POINT ( 'NONE', #9785 ) ;
#2788 = CIRCLE ( 'NONE', #3301, 25.00000000000000000 ) ;
#2789 = VERTEX_POINT ( 'NONE', #3087 ) ;
#2790 = DIRECTION ( 'NONE',  ( 0.000000000000000000, 2.775557561562888270E-17, 1.000000000000000000 ) ) ;
#2791 = DIRECTION ( 'NONE',  ( 0.000000000000000000, -1.000000000000000000, 0.000000000000000000 ) ) ;
#2792 = EDGE_CURVE ( 'NONE', #417, #7784, #6480, .T. ) ;
#2793 = CARTESIAN_POINT ( 'NONE',  ( -24.62111388750000884, 1.956249999044084698, 10.19839929293505421 ) ) ;
#2794 = EDGE_LOOP ( 'NONE', ( #8316, #2222, #2779 ) ) ;
#2795 = EDGE_CURVE ( 'NONE', #2980, #2038, #7977, .T. ) ;
#2796 = CARTESIAN_POINT ( 'NONE',  ( 0.000000000000000000, 85.00000000000000000, 0.000000000000000000 ) ) ;
#2797 = DIRECTION ( 'NONE',  ( -0.000000000000000000, 1.000000000000000000, 0.000000000000000000 ) ) ;
#2798 = DIRECTION ( 'NONE',  ( 0.000000000000000000, 0.000000000000000000, 1.000000000000000000 ) ) ;
#2799 = ADVANCED_FACE ( 'NONE', ( #5652 ), #8659, .F. ) ;
#2800 = ORIENTED_EDGE ( 'NONE', *, *, #7971, .T. ) ;
#2801 = ORIENTED_EDGE ( 'NONE', *, *, #4682, .T. ) ;
#2802 = LINE ( 'NONE', #6204, #1581 ) ;
#2803 = CARTESIAN_POINT ( 'NONE',  ( 0.000000000000000000, 5.000000000000000000, 0.000000000000000000 ) ) ;
#2804 = VECTOR ( 'NONE', #7583, 999.9999999999998863 ) ;
#2805 = CARTESIAN_POINT ( 'NONE',  ( 5.276923788646596947, -0.001000000000001000089, -15.13990010960494459 ) ) ;
#2806 = VERTEX_POINT ( 'NONE', #7842 ) ;
#2807 = EDGE_CURVE ( 'NONE', #10131, #4266, #10239, .T. ) ;
#2808 = DIRECTION ( 'NONE',  ( 0.000000000000000000, 1.000000000000000000, 0.000000000000000000 ) ) ;
#2809 = SURFACE_STYLE_FILL_AREA ( #5155 ) ;
#2810 = CARTESIAN_POINT ( 'NONE',  ( 0.000000000000000000, 10.00000000000000355, 0.000000000000000000 ) ) ;
#2811 = CARTESIAN_POINT ( 'NONE',  ( 24.62111388749999108, 4.156249999044084653, 10.19839929293507730 ) ) ;
#2812 = CARTESIAN_POINT ( 'NONE',  ( 10.35640646055104064, 93.66987298107783033, 5.000000000000000000 ) ) ;
#2813 = ADVANCED_FACE ( 'NONE', ( #7780 ), #2734, .F. ) ;
#2814 = ADVANCED_FACE ( 'NONE', ( #4542 ), #3687, .T. ) ;
#2815 = VECTOR ( 'NONE', #10825, 1000.000000000000000 ) ;
#2816 = EDGE_LOOP ( 'NONE', ( #1467, #3149 ) ) ;
#2817 = VECTOR ( 'NONE', #8387, 1000.000000000000000 ) ;
#2818 = VERTEX_POINT ( 'NONE', #3512 ) ;
#2819 = DIRECTION ( 'NONE',  ( 0.1889822365046095465, -0.000000000000000000, 0.9819805060619665182 ) ) ;
#2820 = CARTESIAN_POINT ( 'NONE',  ( 17.40975659021752975, 2.343749999044085097, -17.40975659021752975 ) ) ;
#2821 = CARTESIAN_POINT ( 'NONE',  ( 0.000000000000000000, 88.00000000000001421, 0.000000000000000000 ) ) ;
#2822 = CARTESIAN_POINT ( 'NONE',  ( 17.67766952966368521, 3.487499998088169129, 17.67766952966369232 ) ) ;
#2823 = CARTESIAN_POINT ( 'NONE',  ( 0.000000000000000000, 10.00000000000000355, 0.000000000000000000 ) ) ;
#2824 = AXIS2_PLACEMENT_3D ( 'NONE', #2561, #5956, #9312 ) ;
#2825 = DIRECTION ( 'NONE',  ( 0.8838834764831863255, -0.3535533905932720100, -0.3061862178478936269 ) ) ;
#2826 = CARTESIAN_POINT ( 'NONE',  ( -25.00000000000001066, 2.562500000000000444, 10.35533905932737397 ) ) ;
#2827 = CARTESIAN_POINT ( 'NONE',  ( 82.32050807568876394, 0.000000000000000000, 0.000000000000000000 ) ) ;
#2828 = CARTESIAN_POINT ( 'NONE',  ( -3.933012701892143692, 10.00000000000000355, -5.812177826491118360 ) ) ;
#2829 = ORIENTED_EDGE ( 'NONE', *, *, #3893, .F. ) ;
#2830 = VERTEX_POINT ( 'NONE', #9435 ) ;
#2831 = ORIENTED_EDGE ( 'NONE', *, *, #5771, .T. ) ;
#2832 = VECTOR ( 'NONE', #7350, 1000.000000000000000 ) ;
#2833 = VECTOR ( 'NONE', #4440, 1000.000000000000000 ) ;
#2834 = CARTESIAN_POINT ( 'NONE',  ( 0.000000000000000000, 7.000000000000003553, 0.000000000000000000 ) ) ;
#2835 = DIRECTION ( 'NONE',  ( 0.8660254037844433705, 0.000000000000000000, 0.4999999999999916733 ) ) ;
#2836 = FACE_OUTER_BOUND ( 'NONE', #2536, .T. ) ;
#2837 = FACE_OUTER_BOUND ( 'NONE', #137, .T. ) ;
#2838 = FACE_OUTER_BOUND ( 'NONE', #5537, .T. ) ;
#2839 = ADVANCED_FACE ( 'NONE', ( #7617 ), #8220, .T. ) ;
#2840 = DIRECTION ( 'NONE',  ( -0.000000000000000000, -0.000000000000000000, 1.000000000000000000 ) ) ;
#2841 = CARTESIAN_POINT ( 'NONE',  ( -10.35533905932737220, 1.687500000000000222, 25.00000000000001421 ) ) ;
#2842 = CARTESIAN_POINT ( 'NONE',  ( -24.62111388750000884, 4.956249999044084475, 10.19839929293505421 ) ) ;
#2843 = AXIS2_PLACEMENT_3D ( 'NONE', #1682, #9961, #803 ) ;
#2844 = ORIENTED_EDGE ( 'NONE', *, *, #3505, .T. ) ;
#2845 = ORIENTED_EDGE ( 'NONE', *, *, #2923, .F. ) ;
#2846 = SURFACE_STYLE_FILL_AREA ( #4545 ) ;
#2847 = AXIS2_PLACEMENT_3D ( 'NONE', #9889, #2642, #3749 ) ;
#2848 = CARTESIAN_POINT ( 'NONE',  ( -10.19839929293505776, 3.706249999044085808, -24.62111388750000174 ) ) ;
#2849 = PLANE ( 'NONE',  #5816 ) ;
#2850 = DIRECTION ( 'NONE',  ( -0.000000000000000000, -1.000000000000000000, -0.000000000000000000 ) ) ;
#2851 = CARTESIAN_POINT ( 'NONE',  ( -5.665063509460962266, 10.00000000000000355, -10.81217782649115122 ) ) ;
#2852 = AXIS2_PLACEMENT_3D ( 'NONE', #7620, #9391, #4320 ) ;
#2853 = AXIS2_PLACEMENT_3D ( 'NONE', #9859, #5677, #10590 ) ;
#2854 = AXIS2_PLACEMENT_3D ( 'NONE', #4009, #3960, #3902 ) ;
#2855 = VERTEX_POINT ( 'NONE', #9065 ) ;
#2856 = EDGE_CURVE ( 'NONE', #2446, #2130, #5828, .T. ) ;
#2857 = CIRCLE ( 'NONE', #4995, 4.999999999999997335 ) ;
#2858 = VECTOR ( 'NONE', #10634, 1000.000000000000000 ) ;
#2859 = CARTESIAN_POINT ( 'NONE',  ( 27.60306914047445304, 97.85373563005803987, 5.000000000000000000 ) ) ;
#2860 = CARTESIAN_POINT ( 'NONE',  ( -17.67766952966368876, 0.3750000000000000000, -17.67766952966369232 ) ) ;
#2861 = LINE ( 'NONE', #3706, #5351 ) ;
#2862 = VERTEX_POINT ( 'NONE', #6525 ) ;
#2863 = DIRECTION ( 'NONE',  ( -0.6546536707079774198, 0.000000000000000000, -0.7559289460184541731 ) ) ;
#2864 = EDGE_CURVE ( 'NONE', #10373, #10312, #9709, .T. ) ;
#2865 = CARTESIAN_POINT ( 'NONE',  ( 1.040834085586084257E-14, 88.00000000000001421, 0.000000000000000000 ) ) ;
#2866 = VECTOR ( 'NONE', #9292, 1000.000000000000000 ) ;
#2867 = CARTESIAN_POINT ( 'NONE',  ( 1.507608415688466075E-15, 4.468749999044084653, -24.62111388750000174 ) ) ;
#2868 = CARTESIAN_POINT ( 'NONE',  ( 17.67766952966368521, 2.487499998088169129, 17.67766952966369232 ) ) ;
#2869 =( BOUNDED_CURVE ( )  B_SPLINE_CURVE ( 3, ( #7760, #4573, #354, #6113 ),
 .UNSPECIFIED., .F., .F. ) 
 B_SPLINE_CURVE_WITH_KNOTS ( ( 4, 4 ),
 ( 3.927175151554400223, 3.998664601439921640 ),
 .UNSPECIFIED. ) 
 CURVE ( )  GEOMETRIC_REPRESENTATION_ITEM ( )  RATIONAL_B_SPLINE_CURVE ( ( 1.000000000000000000, 0.9995741502243209453, 0.9995741502243209453, 1.000000000000000000 ) ) 
 REPRESENTATION_ITEM ( '' )  );
#2870 = MECHANICAL_DESIGN_GEOMETRIC_PRESENTATION_REPRESENTATION (  '', ( #5521 ), #1640 ) ;
#2871 = CIRCLE ( 'NONE', #8166, 2.999999999999997780 ) ;
#2872 = ORIENTED_EDGE ( 'NONE', *, *, #2573, .T. ) ;
#2873 = EDGE_CURVE ( 'NONE', #1851, #5761, #7455, .T. ) ;
#2874 = VECTOR ( 'NONE', #9459, 1000.000000000000000 ) ;
#2875 = CARTESIAN_POINT ( 'NONE',  ( 1.530808498934191521E-15, 0.2500000000000000000, -25.00000000000000000 ) ) ;
#2876 = CARTESIAN_POINT ( 'NONE',  ( -24.62111388750000174, 2.656249999044085097, -10.19839929293506131 ) ) ;
#2877 = CARTESIAN_POINT ( 'NONE',  ( 1.507608415688466075E-15, 4.643749999044085364, -24.62111388750000174 ) ) ;
#2878 = AXIS2_PLACEMENT_3D ( 'NONE', #982, #10255, #9192 ) ;
#2879 = CARTESIAN_POINT ( 'NONE',  ( -4.592425496802574367E-15, 2.750000000000000000, 25.00000000000000000 ) ) ;
#2880 = ADVANCED_FACE ( 'NONE', ( #9881 ), #1084, .T. ) ;
#2881 = FACE_OUTER_BOUND ( 'NONE', #8570, .T. ) ;
#2882 = FACE_BOUND ( 'NONE', #10230, .T. ) ;
#2883 = DIRECTION ( 'NONE',  ( 0.000000000000000000, -1.000000000000000000, 0.000000000000000000 ) ) ;
#2884 = DIRECTION ( 'NONE',  ( 0.000000000000000000, -0.000000000000000000, -1.000000000000000000 ) ) ;
#2885 = VECTOR ( 'NONE', #9447, 1000.000000000000000 ) ;
#2886 = VERTEX_POINT ( 'NONE', #5801 ) ;
#2887 = CARTESIAN_POINT ( 'NONE',  ( 0.000000000000000000, 20.00000000000000355, 0.000000000000000000 ) ) ;
#2888 = ADVANCED_FACE ( 'NONE', ( #6632 ), #10717, .T. ) ;
#2889 = DIRECTION ( 'NONE',  ( -0.000000000000000000, 1.000000000000000000, 0.000000000000000000 ) ) ;
#2890 = FACE_OUTER_BOUND ( 'NONE', #6042, .T. ) ;
#2891 = CARTESIAN_POINT ( 'NONE',  ( -9.874999999999777955, -0.001000000000001000089, 17.10400172474279401 ) ) ;
#2892 = DIRECTION ( 'NONE',  ( -1.000000000000000000, -2.775557561562888984E-15, 0.000000000000000000 ) ) ;
#2893 = CARTESIAN_POINT ( 'NONE',  ( -17.10400172474275848, -0.001000000000001000089, -9.874999999999836575 ) ) ;
#2894 = ORIENTED_EDGE ( 'NONE', *, *, #10331, .F. ) ;
#2895 = ORIENTED_EDGE ( 'NONE', *, *, #3220, .F. ) ;
#2896 = PRODUCT_DEFINITION_SHAPE ( 'NONE', 'NONE',  #14 ) ;
#2897 = DIRECTION ( 'NONE',  ( -0.7559289460184582810, 0.000000000000000000, 0.6546536707079726458 ) ) ;
#2898 = DIRECTION ( 'NONE',  ( -0.8660254037844432595, 0.000000000000000000, 0.4999999999999919509 ) ) ;
#2899 = CARTESIAN_POINT ( 'NONE',  ( -6.982120021884462346, 19.03096903053432243, -0.5000000000000731637 ) ) ;
#2900 = DIRECTION ( 'NONE',  ( -0.8660254037844361541, 0.000000000000000000, 0.5000000000000042188 ) ) ;
#2901 = DIRECTION ( 'NONE',  ( 0.000000000000000000, 0.000000000000000000, 1.000000000000000000 ) ) ;
#2902 = EDGE_LOOP ( 'NONE', ( #2577, #5014, #4778, #990 ) ) ;
#2903 = ORIENTED_EDGE ( 'NONE', *, *, #3124, .F. ) ;
#2904 = CARTESIAN_POINT ( 'NONE',  ( -4.522825247065398226E-15, 5.143749999044084475, 24.62111388750000174 ) ) ;
#2905 = DIRECTION ( 'NONE',  ( 0.000000000000000000, 0.000000000000000000, -1.000000000000000000 ) ) ;
#2906 = DIRECTION ( 'NONE',  ( -1.000000000000000000, 0.000000000000000000, 0.000000000000000000 ) ) ;
#2907 = CARTESIAN_POINT ( 'NONE',  ( 6.223805082245728038, 19.34316356887878285, 3.208128317448950551 ) ) ;
#2908 = ORIENTED_EDGE ( 'NONE', *, *, #6868, .F. ) ;
#2909 = DIRECTION ( 'NONE',  ( 1.000000000000000000, 0.000000000000000000, 0.000000000000000000 ) ) ;
#2910 = FACE_BOUND ( 'NONE', #7286, .T. ) ;
#2911 = ORIENTED_EDGE ( 'NONE', *, *, #4602, .F. ) ;
#2912 = CARTESIAN_POINT ( 'NONE',  ( 10.19839929293506486, 4.031249999044083765, 24.62111388749999819 ) ) ;
#2913 = CARTESIAN_POINT ( 'NONE',  ( -6.062177826491028654, 20.00000000000000355, -3.500000000000069722 ) ) ;
#2914 = EDGE_CURVE ( 'NONE', #10312, #7767, #6475, .T. ) ;
#2915 = ORIENTED_EDGE ( 'NONE', *, *, #3317, .F. ) ;
#2916 = ORIENTED_EDGE ( 'NONE', *, *, #1066, .T. ) ;
#2917 = ORIENTED_EDGE ( 'NONE', *, *, #9280, .F. ) ;
#2918 = DIRECTION ( 'NONE',  ( -0.000000000000000000, 1.000000000000000000, -0.000000000000000000 ) ) ;
#2919 = CARTESIAN_POINT ( 'NONE',  ( -17.40975659021752975, 3.593749999044084653, -17.40975659021752975 ) ) ;
#2920 = CARTESIAN_POINT ( 'NONE',  ( 17.40975659021752975, 3.518749999044084920, -17.40975659021752975 ) ) ;
#2921 = CARTESIAN_POINT ( 'NONE',  ( -25.00000000000000000, 4.500000000000000888, -3.061616997868383043E-15 ) ) ;
#2922 = PRESENTATION_STYLE_ASSIGNMENT (( #6478 ) ) ;
#2923 = EDGE_CURVE ( 'NONE', #9832, #514, #3131, .T. ) ;
#2924 =( BOUNDED_CURVE ( )  B_SPLINE_CURVE ( 3, ( #4047, #8346, #5651, #9946 ),
 .UNSPECIFIED., .F., .F. ) 
 B_SPLINE_CURVE_WITH_KNOTS ( ( 4, 4 ),
 ( 3.927175151554404664, 3.998664601439924748 ),
 .UNSPECIFIED. ) 
 CURVE ( )  GEOMETRIC_REPRESENTATION_ITEM ( )  RATIONAL_B_SPLINE_CURVE ( ( 1.000000000000000000, 0.9995741502243209453, 0.9995741502243209453, 1.000000000000000000 ) ) 
 REPRESENTATION_ITEM ( '' )  );
#2925 = EDGE_CURVE ( 'NONE', #6596, #2139, #5480, .T. ) ;
#2926 = DIRECTION ( 'NONE',  ( -0.5000000000000009992, 0.8660254037844380415, -1.745740669421570228E-15 ) ) ;
#2927 = CARTESIAN_POINT ( 'NONE',  ( 17.67766952966369232, 0.7374999980881691286, -17.67766952966369232 ) ) ;
#2928 = CYLINDRICAL_SURFACE ( 'NONE', #3187, 5.000000000000004441 ) ;
#2929 = CARTESIAN_POINT ( 'NONE',  ( 0.000000000000000000, -8.000000000000000000, 0.000000000000000000 ) ) ;
#2930 = EDGE_LOOP ( 'NONE', ( #9824, #2494, #5538, #1927 ) ) ;
#2931 = VERTEX_POINT ( 'NONE', #4150 ) ;
#2932 = EDGE_CURVE ( 'NONE', #5856, #1858, #6581, .T. ) ;
#2933 = VERTEX_POINT ( 'NONE', #4984 ) ;
#2934 = DIRECTION ( 'NONE',  ( -0.000000000000000000, 1.000000000000000000, -0.000000000000000000 ) ) ;
#2935 = AXIS2_PLACEMENT_3D ( 'NONE', #3896, #10686, #2226 ) ;
#2936 = CARTESIAN_POINT ( 'NONE',  ( 0.000000000000000000, 20.00000000000000355, 0.000000000000000000 ) ) ;
#2937 = ADVANCED_FACE ( 'NONE', ( #9829 ), #10776, .F. ) ;
#2938 = FACE_OUTER_BOUND ( 'NONE', #4343, .T. ) ;
#2939 = FACE_OUTER_BOUND ( 'NONE', #7223, .T. ) ;
#2940 = CYLINDRICAL_SURFACE ( 'NONE', #7785, 6.999999999999997335 ) ;
#2941 = FACE_OUTER_BOUND ( 'NONE', #10377, .T. ) ;
#2942 = VERTEX_POINT ( 'NONE', #8122 ) ;
#2943 = EDGE_CURVE ( 'NONE', #1427, #10373, #2419, .T. ) ;
#2944 = PRESENTATION_LAYER_ASSIGNMENT (  '', '', ( #7728 ) ) ;
#2945 = EDGE_LOOP ( 'NONE', ( #515, #488, #82, #2456 ) ) ;
#2946 = AXIS2_PLACEMENT_3D ( 'NONE', #3941, #509, #7198 ) ;
#2947 = LINE ( 'NONE', #7217, #10623 ) ;
#2948 = CARTESIAN_POINT ( 'NONE',  ( 0.000000000000000000, 5.000000000000000000, -25.00000000000000000 ) ) ;
#2949 = LINE ( 'NONE', #7219, #7293 ) ;
#2950 = CARTESIAN_POINT ( 'NONE',  ( 25.00000000000000000, 5.000000000000000000, 0.000000000000000000 ) ) ;
#2951 = DIRECTION ( 'NONE',  ( 0.000000000000000000, 1.000000000000000000, 0.000000000000000000 ) ) ;
#2952 = CIRCLE ( 'NONE', #5794, 5.525000000000006573 ) ;
#2953 = ORIENTED_EDGE ( 'NONE', *, *, #6071, .F. ) ;
#2954 = DIRECTION ( 'NONE',  ( 0.000000000000000000, 1.000000000000000000, 0.000000000000000000 ) ) ;
#2955 = DIRECTION ( 'NONE',  ( 0.000000000000000000, 1.000000000000000000, 0.000000000000000000 ) ) ;
#2956 = CARTESIAN_POINT ( 'NONE',  ( -24.62111388750000174, 4.831249999044084475, -10.19839929293506131 ) ) ;
#2957 = ORIENTED_EDGE ( 'NONE', *, *, #6201, .F. ) ;
#2958 = DIRECTION ( 'NONE',  ( 0.000000000000000000, -1.000000000000000000, 0.000000000000000000 ) ) ;
#2959 = FILL_AREA_STYLE ('',( #5582 ) ) ;
#2960 = CARTESIAN_POINT ( 'NONE',  ( 15.60400172474269453, -0.001000000000001000089, 12.47307621135327693 ) ) ;
#2961 = ORIENTED_EDGE ( 'NONE', *, *, #10313, .T. ) ;
#2962 = CARTESIAN_POINT ( 'NONE',  ( -17.40975659021753330, 1.843749999044084653, 17.40975659021752975 ) ) ;
#2963 = DIRECTION ( 'NONE',  ( 0.000000000000000000, 0.8660254037844380415, -0.5000000000000009992 ) ) ;
#2964 = ORIENTED_EDGE ( 'NONE', *, *, #7197, .T. ) ;
#2965 = VERTEX_POINT ( 'NONE', #5700 ) ;
#2966 = ORIENTED_EDGE ( 'NONE', *, *, #1680, .T. ) ;
#2967 = PRODUCT_RELATED_PRODUCT_CATEGORY ( 'part', '', ( #10587 ) ) ;
#2968 = CARTESIAN_POINT ( 'NONE',  ( 17.67766952966369232, 1.737499998088169351, -17.67766952966369232 ) ) ;
#2969 = DIRECTION ( 'NONE',  ( 0.000000000000000000, 0.000000000000000000, 1.000000000000000000 ) ) ;
#2970 = CARTESIAN_POINT ( 'NONE',  ( 24.62111388750000174, 1.218749999044084431, 0.000000000000000000 ) ) ;
#2971 = CARTESIAN_POINT ( 'NONE',  ( 24.62111388750000174, 3.393749999044084475, 0.000000000000000000 ) ) ;
#2972 = VERTEX_POINT ( 'NONE', #8952 ) ;
#2973 = CARTESIAN_POINT ( 'NONE',  ( 24.99999999999999289, 1.937500000000000000, 10.35533905932739529 ) ) ;
#2974 = CARTESIAN_POINT ( 'NONE',  ( 2.500000000000000444, 1.000000000000001998, 0.5773502691896277295 ) ) ;
#2975 = CARTESIAN_POINT ( 'NONE',  ( -25.00000000000000000, 1.049999998088169129, -10.35533905932738108 ) ) ;
#2976 = FACE_OUTER_BOUND ( 'NONE', #7574, .T. ) ;
#2977 = CARTESIAN_POINT ( 'NONE',  ( 25.00000000000000000, 1.000000000000000000, 0.000000000000000000 ) ) ;
#2978 = AXIS2_PLACEMENT_3D ( 'NONE', #9100, #6680, #10880 ) ;
#2979 = AXIS2_PLACEMENT_3D ( 'NONE', #10058, #4993, #3242 ) ;
#2980 = VERTEX_POINT ( 'NONE', #7510 ) ;
#2981 = ORIENTED_EDGE ( 'NONE', *, *, #8651, .T. ) ;
#2982 = ORIENTED_EDGE ( 'NONE', *, *, #2078, .F. ) ;
#2983 = ORIENTED_EDGE ( 'NONE', *, *, #2250, .T. ) ;
#2984 = EDGE_CURVE ( 'NONE', #6236, #1658, #4434, .T. ) ;
#2985 = CARTESIAN_POINT ( 'NONE',  ( -15.75000000000000000, 28.00000000000000000, 1.681956355172181189E-13 ) ) ;
#2986 = CIRCLE ( 'NONE', #8460, 2.999999999999997335 ) ;
#2987 = AXIS2_PLACEMENT_3D ( 'NONE', #4656, #1274, #3760 ) ;
#2988 =( BOUNDED_CURVE ( )  B_SPLINE_CURVE ( 2, ( #3954, #10684, #7305, #3093, #568, #8116, #9625, #2100, #4712 ),
 .UNSPECIFIED., .F., .F. ) 
 B_SPLINE_CURVE_WITH_KNOTS ( ( 3, 2, 2, 2, 3 ),
 ( 0.7500000000000000000, 0.7750000000000000222, 0.8000000000000000444, 0.8250000000000000666, 0.8500000000000000888 ),
 .UNSPECIFIED. ) 
 CURVE ( )  GEOMETRIC_REPRESENTATION_ITEM ( )  RATIONAL_B_SPLINE_CURVE ( ( 1.000000000000000000, 0.9238795325112867385, 1.000000000000000000, 0.9238795325112867385, 1.000000000000000000, 0.9238795325112867385, 1.000000000000000000, 0.9238795325112864054, 1.000000000000000444 ) ) 
 REPRESENTATION_ITEM ( '' )  );
#2989 = CARTESIAN_POINT ( 'NONE',  ( 0.000000000000000000, 20.00000000000000355, 20.00000000000000000 ) ) ;
#2990 = DIRECTION ( 'NONE',  ( 0.000000000000000000, 1.000000000000000000, -1.502202555303642096E-16 ) ) ;
#2991 = EDGE_LOOP ( 'NONE', ( #6706, #7409 ) ) ;
#2992 = FACE_OUTER_BOUND ( 'NONE', #8759, .T. ) ;
#2993 = ADVANCED_FACE ( 'NONE', ( #9005 ), #10671, .T. ) ;
#2994 = CARTESIAN_POINT ( 'NONE',  ( 0.000000000000000000, 85.00000000000000000, 0.000000000000000000 ) ) ;
#2995 = FACE_OUTER_BOUND ( 'NONE', #5402, .T. ) ;
#2996 = CARTESIAN_POINT ( 'NONE',  ( -3.058047309050066165, 10.00000000000000355, 6.296693311223885203 ) ) ;
#2997 = AXIS2_PLACEMENT_3D ( 'NONE', #10423, #8870, #6242 ) ;
#2998 = VECTOR ( 'NONE', #7666, 1000.000000000000000 ) ;
#2999 = ADVANCED_FACE ( 'NONE', ( #7295 ), #8181, .F. ) ;
#3000 = ORIENTED_EDGE ( 'NONE', *, *, #5404, .T. ) ;
#3001 = DIRECTION ( 'NONE',  ( 0.000000000000000000, 0.9848077530122080203, 0.1736481776669307198 ) ) ;
#3002 = FACE_OUTER_BOUND ( 'NONE', #6915, .T. ) ;
#3003 = EDGE_CURVE ( 'NONE', #10544, #8354, #53, .T. ) ;
#3004 = DIRECTION ( 'NONE',  ( 0.8660254037844363761, 0.000000000000000000, 0.5000000000000039968 ) ) ;
#3005 = AXIS2_PLACEMENT_3D ( 'NONE', #7212, #10580, #2286 ) ;
#3006 = FACE_OUTER_BOUND ( 'NONE', #6313, .T. ) ;
#3007 = DIRECTION ( 'NONE',  ( 2.126576849575776229E-17, 0.9848077530122080203, -0.1736481776669307198 ) ) ;
#3008 = ORIENTED_EDGE ( 'NONE', *, *, #8939, .T. ) ;
#3009 = ORIENTED_EDGE ( 'NONE', *, *, #2923, .T. ) ;
#3010 = VECTOR ( 'NONE', #8186, 1000.000000000000000 ) ;
#3011 = CARTESIAN_POINT ( 'NONE',  ( -19.74999999999996803, 25.00000000000000000, 3.000000000000206057 ) ) ;
#3012 = CARTESIAN_POINT ( 'NONE',  ( 1.530808498934191521E-15, 0.2500000000000000000, -25.00000000000000000 ) ) ;
#3013 = CARTESIAN_POINT ( 'NONE',  ( 19.75000000000001066, -0.001000000000001000089, 2.999999999999927613 ) ) ;
#3014 = EDGE_CURVE ( 'NONE', #849, #2806, #10214, .T. ) ;
#3015 = EDGE_LOOP ( 'NONE', ( #10006, #2344, #5681, #10885 ) ) ;
#3016 = CYLINDRICAL_SURFACE ( 'NONE', #1788, 6.999999999999997335 ) ;
#3017 = SURFACE_STYLE_FILL_AREA ( #2959 ) ;
#3018 = DIRECTION ( 'NONE',  ( 0.000000000000000000, 0.000000000000000000, 1.000000000000000000 ) ) ;
#3019 = ORIENTED_EDGE ( 'NONE', *, *, #2384, .F. ) ;
#3020 = CARTESIAN_POINT ( 'NONE',  ( -17.40975659021752975, 2.593749999044084653, -17.40975659021752975 ) ) ;
#3021 = CARTESIAN_POINT ( 'NONE',  ( -0.5000000000000000000, 19.74999999999999645, 6.566987298107768822 ) ) ;
#3022 = AXIS2_PLACEMENT_3D ( 'NONE', #10322, #1869, #5412 ) ;
#3023 = ORIENTED_EDGE ( 'NONE', *, *, #9075, .F. ) ;
#3024 = ORIENTED_EDGE ( 'NONE', *, *, #9227, .F. ) ;
#3025 = VECTOR ( 'NONE', #6122, 999.9999999999998863 ) ;
#3026 = ORIENTED_EDGE ( 'NONE', *, *, #9765, .T. ) ;
#3027 = VECTOR ( 'NONE', #10579, 1000.000000000000000 ) ;
#3028 = CARTESIAN_POINT ( 'NONE',  ( -10.35533905932739174, 4.299999998088169129, 24.99999999999999289 ) ) ;
#3029 = CARTESIAN_POINT ( 'NONE',  ( -4.522825247065398226E-15, 4.968749999044083765, 24.62111388750000174 ) ) ;
#3030 = VECTOR ( 'NONE', #5335, 1000.000000000000114 ) ;
#3031 = CARTESIAN_POINT ( 'NONE',  ( 1.507608415688466075E-15, 2.643749999044084920, -24.62111388750000174 ) ) ;
#3032 = CARTESIAN_POINT ( 'NONE',  ( -17.67766952966368876, 2.375000000000000000, -17.67766952966369232 ) ) ;
#3033 = DIRECTION ( 'NONE',  ( 1.000000000000000000, 0.000000000000000000, -2.168404344971010347E-16 ) ) ;
#3034 = VECTOR ( 'NONE', #8788, 1000.000000000000114 ) ;
#3035 = DIRECTION ( 'NONE',  ( -0.5000000000000069944, 0.000000000000000000, 0.8660254037844344888 ) ) ;
#3036 = CARTESIAN_POINT ( 'NONE',  ( -12.47307621135344391, 28.00000000000000000, -15.60400172474256131 ) ) ;
#3037 = VECTOR ( 'NONE', #3855, 1000.000000000000000 ) ;
#3038 = FACE_OUTER_BOUND ( 'NONE', #9876, .T. ) ;
#3039 = VERTEX_POINT ( 'NONE', #5263 ) ;
#3040 = ORIENTED_EDGE ( 'NONE', *, *, #5386, .F. ) ;
#3041 = UNCERTAINTY_MEASURE_WITH_UNIT (LENGTH_MEASURE( 1.000000000000000082E-05 ), #5577, 'distance_accuracy_value', 'NONE');
#3042 = CARTESIAN_POINT ( 'NONE',  ( -17.67766952966369232, 0.6250000000000000000, 17.67766952966368876 ) ) ;
#3043 = CARTESIAN_POINT ( 'NONE',  ( -25.00000000000001066, 4.562500000000001776, 10.35533905932737397 ) ) ;
#3044 = DIRECTION ( 'NONE',  ( -0.000000000000000000, 1.000000000000000000, 0.000000000000000000 ) ) ;
#3045 = CARTESIAN_POINT ( 'NONE',  ( 0.000000000000000000, -4.336808689942017736E-16, 1.154700538379254571 ) ) ;
#3046 = CARTESIAN_POINT ( 'NONE',  ( 2.500000000000000444, -1.000000000000003331, 0.5773502691896272854 ) ) ;
#3047 = PRODUCT_RELATED_PRODUCT_CATEGORY ( 'part', '', ( #6284 ) ) ;
#3048 = EDGE_CURVE ( 'NONE', #956, #10147, #3155, .T. ) ;
#3049 = LINE ( 'NONE', #9650, #9000 ) ;
#3050 = DIRECTION ( 'NONE',  ( 0.000000000000000000, 0.000000000000000000, 1.000000000000000000 ) ) ;
#3051 = VERTEX_POINT ( 'NONE', #10280 ) ;
#3052 = VERTEX_POINT ( 'NONE', #6804 ) ;
#3053 = ORIENTED_EDGE ( 'NONE', *, *, #1199, .F. ) ;
#3054 =( BOUNDED_CURVE ( )  B_SPLINE_CURVE ( 2, ( #9773, #10451, #1330, #6368, #8061 ),
 .UNSPECIFIED., .F., .F. ) 
 B_SPLINE_CURVE_WITH_KNOTS ( ( 3, 2, 3 ),
 ( 0.000000000000000000, 0.02500000000000000486, 0.05000000000000000971 ),
 .UNSPECIFIED. ) 
 CURVE ( )  GEOMETRIC_REPRESENTATION_ITEM ( )  RATIONAL_B_SPLINE_CURVE ( ( 1.000000000000000000, 0.9238795325112867385, 1.000000000000000000, 0.9238795325112867385, 1.000000000000000000 ) ) 
 REPRESENTATION_ITEM ( '' )  );
#3055 = EDGE_CURVE ( 'NONE', #6443, #3821, #9868, .T. ) ;
#3056 = ORIENTED_EDGE ( 'NONE', *, *, #921, .F. ) ;
#3057 = FACE_OUTER_BOUND ( 'NONE', #7326, .T. ) ;
#3058 = DIRECTION ( 'NONE',  ( -0.000000000000000000, 0.000000000000000000, -1.000000000000000000 ) ) ;
#3059 = CARTESIAN_POINT ( 'NONE',  ( 25.00000000000000000, 4.612499998088169129, 0.000000000000000000 ) ) ;
#3060 = EDGE_CURVE ( 'NONE', #3974, #3699, #7736, .T. ) ;
#3061 = CARTESIAN_POINT ( 'NONE',  ( 25.00000000000000000, 1.062500000000000222, -10.35533905932737753 ) ) ;
#3062 = EDGE_CURVE ( 'NONE', #10429, #544, #9265, .T. ) ;
#3063 = FACE_OUTER_BOUND ( 'NONE', #2015, .T. ) ;
#3064 = ADVANCED_FACE ( 'NONE', ( #9322 ), #4318, .F. ) ;
#3065 = ORIENTED_EDGE ( 'NONE', *, *, #5471, .T. ) ;
#3066 = EDGE_CURVE ( 'NONE', #5286, #1765, #9349, .T. ) ;
#3067 = VERTEX_POINT ( 'NONE', #5916 ) ;
#3068 = DIRECTION ( 'NONE',  ( 0.000000000000000000, 1.000000000000000000, 0.000000000000000000 ) ) ;
#3069 = CARTESIAN_POINT ( 'NONE',  ( -4.522825247065398226E-15, 4.143749999044083587, 24.62111388750000174 ) ) ;
#3070 = ORIENTED_EDGE ( 'NONE', *, *, #4644, .T. ) ;
#3071 = CARTESIAN_POINT ( 'NONE',  ( 66.68467533811312364, 89.45240317130979690, 5.000000000000000000 ) ) ;
#3072 = SURFACE_STYLE_FILL_AREA ( #5529 ) ;
#3073 = DIRECTION ( 'NONE',  ( 0.000000000000000000, -0.8660254037844387076, 0.4999999999999999445 ) ) ;
#3074 = ORIENTED_EDGE ( 'NONE', *, *, #8684, .T. ) ;
#3075 = DIRECTION ( 'NONE',  ( 0.4330127018922226290, 0.8660254037844380415, -0.2499999999999965028 ) ) ;
#3076 = EDGE_CURVE ( 'NONE', #2342, #1227, #6858, .T. ) ;
#3077 = CARTESIAN_POINT ( 'NONE',  ( 1.400000000000001910, -1.387778780781445676E-16, -5.000000000000005329 ) ) ;
#3078 = VERTEX_POINT ( 'NONE', #6030 ) ;
#3079 = EDGE_LOOP ( 'NONE', ( #4222, #5495, #8353, #1863 ) ) ;
#3080 = EDGE_CURVE ( 'NONE', #4640, #8585, #9217, .T. ) ;
#3081 = CARTESIAN_POINT ( 'NONE',  ( 1.530808498934191521E-15, 2.862499998088169573, -25.00000000000000000 ) ) ;
#3082 = CARTESIAN_POINT ( 'NONE',  ( 15.60400172474269453, 28.00000000000000000, 12.47307621135327693 ) ) ;
#3083 = CARTESIAN_POINT ( 'NONE',  ( -24.62111388750000174, 1.718749999044084431, -3.015216831376932151E-15 ) ) ;
#3084 = ORIENTED_EDGE ( 'NONE', *, *, #6791, .F. ) ;
#3085 = CARTESIAN_POINT ( 'NONE',  ( -19.74999999999996803, -0.001000000000001000089, 3.000000000000206057 ) ) ;
#3086 = DIRECTION ( 'NONE',  ( -0.5000000000000073275, 0.000000000000000000, -0.8660254037844343777 ) ) ;
#3087 = CARTESIAN_POINT ( 'NONE',  ( -1.500000000000001776, 7.661233032048582725E-16, 5.100000000000006750 ) ) ;
#3088 = FACE_OUTER_BOUND ( 'NONE', #5636, .T. ) ;
#3089 = CARTESIAN_POINT ( 'NONE',  ( -4.592425496802574367E-15, 3.362499998088169129, 25.00000000000000000 ) ) ;
#3090 = ORIENTED_EDGE ( 'NONE', *, *, #574, .T. ) ;
#3091 = ORIENTED_EDGE ( 'NONE', *, *, #3837, .T. ) ;
#3092 = ORIENTED_EDGE ( 'NONE', *, *, #5873, .F. ) ;
#3093 = CARTESIAN_POINT ( 'NONE',  ( 24.99999999999999289, 3.937500000000000000, 10.35533905932739529 ) ) ;
#3094 = CARTESIAN_POINT ( 'NONE',  ( -1.500000000000001332, 0.000000000000000000, 0.000000000000000000 ) ) ;
#3095 =( NAMED_UNIT ( * ) SI_UNIT ( $, .STERADIAN. ) SOLID_ANGLE_UNIT ( ) );
#3096 = CARTESIAN_POINT ( 'NONE',  ( 82.32050807568876394, 99.93473594742127375, -5.349378127920655146 ) ) ;
#3097 = CARTESIAN_POINT ( 'NONE',  ( 0.000000000000000000, 10.00000000000000355, 0.000000000000000000 ) ) ;
#3098 = CARTESIAN_POINT ( 'NONE',  ( -17.40975659021752975, 0.5937499990440846531, -17.40975659021752975 ) ) ;
#3099 = CARTESIAN_POINT ( 'NONE',  ( 1.400000000000001910, 7.586122904283394383E-16, 5.000000000000000000 ) ) ;
#3100 = VERTEX_POINT ( 'NONE', #5089 ) ;
#3101 = EDGE_LOOP ( 'NONE', ( #3790, #360, #8467, #8814 ) ) ;
#3102 = EDGE_LOOP ( 'NONE', ( #5975, #4471, #7632, #808 ) ) ;
#3103 = FACE_OUTER_BOUND ( 'NONE', #5298, .T. ) ;
#3104 = CARTESIAN_POINT ( 'NONE',  ( -10.47307621135341904, 25.00000000000000000, -12.13990010960482557 ) ) ;
#3105 = CARTESIAN_POINT ( 'NONE',  ( 24.62111388750000174, 5.306249999044084120, 0.000000000000000000 ) ) ;
#3106 = CARTESIAN_POINT ( 'NONE',  ( 1.530808498934191521E-15, 0.2500000000000000000, -25.00000000000000000 ) ) ;
#3107 = FACE_OUTER_BOUND ( 'NONE', #8921, .T. ) ;
#3108 = VECTOR ( 'NONE', #9442, 1000.000000000000000 ) ;
#3109 = VECTOR ( 'NONE', #7730, 1000.000000000000000 ) ;
#3110 = EDGE_LOOP ( 'NONE', ( #3092, #10508, #4136, #10819 ) ) ;
#3111 = ADVANCED_FACE ( 'NONE', ( #1660, #7561 ), #1773, .F. ) ;
#3112 = CARTESIAN_POINT ( 'NONE',  ( 0.000000000000000000, 8.000000000000000000, 0.000000000000000000 ) ) ;
#3113 = VECTOR ( 'NONE', #9287, 1000.000000000000000 ) ;
#3114 = CARTESIAN_POINT ( 'NONE',  ( -1.500000000000000444, 83.00000000000000000, 1.499999999999999778 ) ) ;
#3115 = CARTESIAN_POINT ( 'NONE',  ( 10.19839929293505953, 4.581249999044083587, -24.62111388750000174 ) ) ;
#3116 = ORIENTED_EDGE ( 'NONE', *, *, #9145, .T. ) ;
#3117 = CARTESIAN_POINT ( 'NONE',  ( -0.1920286436967143240, 6.605960024862680574E-16, -6.975000000000007638 ) ) ;
#3118 = APPLICATION_PROTOCOL_DEFINITION ( 'draft international standard', 'automotive_design', 1998, #8794 ) ;
#3119 =( REPRESENTATION_RELATIONSHIP ('NONE','NONE', #1269, #9997 ) REPRESENTATION_RELATIONSHIP_WITH_TRANSFORMATION ( #6917 )SHAPE_REPRESENTATION_RELATIONSHIP( ) );
#3120 = LINE ( 'NONE', #4814, #10645 ) ;
#3121 = ORIENTED_EDGE ( 'NONE', *, *, #5395, .F. ) ;
#3122 = VECTOR ( 'NONE', #9223, 1000.000000000000000 ) ;
#3123 = CARTESIAN_POINT ( 'NONE',  ( 1.040834085586084257E-14, 90.00000000000001421, -4.999999999999987566 ) ) ;
#3124 = EDGE_CURVE ( 'NONE', #1765, #5286, #6906, .T. ) ;
#3125 = VERTEX_POINT ( 'NONE', #5214 ) ;
#3126 = VERTEX_POINT ( 'NONE', #3350 ) ;
#3127 = ORIENTED_EDGE ( 'NONE', *, *, #9759, .F. ) ;
#3128 = VECTOR ( 'NONE', #8401, 1000.000000000000000 ) ;
#3129 = EDGE_CURVE ( 'NONE', #2572, #3847, #8119, .T. ) ;
#3130 = CARTESIAN_POINT ( 'NONE',  ( 24.62111388750000174, 0.3937499990440845310, 0.000000000000000000 ) ) ;
#3131 = LINE ( 'NONE', #663, #885 ) ;
#3132 = CARTESIAN_POINT ( 'NONE',  ( -24.62111388750000174, 3.656249999044084653, -10.19839929293506131 ) ) ;
#3133 = ORIENTED_EDGE ( 'NONE', *, *, #2336, .F. ) ;
#3134 = CARTESIAN_POINT ( 'NONE',  ( 1.500000000000001776, 7.661233032048582725E-16, 5.100000000000006750 ) ) ;
#3135 = DIRECTION ( 'NONE',  ( -0.000000000000000000, 1.000000000000000000, -0.000000000000000000 ) ) ;
#3136 = DIRECTION ( 'NONE',  ( 0.000000000000000000, 1.000000000000000000, 0.000000000000000000 ) ) ;
#3137 = DIRECTION ( 'NONE',  ( 0.000000000000000000, -0.8660254037844380415, -0.5000000000000009992 ) ) ;
#3138 = CARTESIAN_POINT ( 'NONE',  ( 24.62111388750000174, 0.3937499990440845310, 0.000000000000000000 ) ) ;
#3139 = ADVANCED_FACE ( 'NONE', ( #8557, #4436 ), #9453, .T. ) ;
#3140 = ORIENTED_EDGE ( 'NONE', *, *, #7546, .T. ) ;
#3141 = EDGE_LOOP ( 'NONE', ( #6644, #3675, #8996 ) ) ;
#3142 =( BOUNDED_CURVE ( )  B_SPLINE_CURVE ( 2, ( #7724, #8430, #9313, #5137, #3579, #9253, #6020, #1646, #6843 ),
 .UNSPECIFIED., .F., .F. ) 
 B_SPLINE_CURVE_WITH_KNOTS ( ( 3, 2, 2, 2, 3 ),
 ( 0.8500000000000000888, 0.8750000000000001110, 0.9000000000000001332, 0.9250000000000001554, 0.9500000000000000666 ),
 .UNSPECIFIED. ) 
 CURVE ( )  GEOMETRIC_REPRESENTATION_ITEM ( )  RATIONAL_B_SPLINE_CURVE ( ( 0.9999999999999996669, 0.9238795325112870716, 1.000000000000000000, 0.9238795325112867385, 1.000000000000000000, 0.9238795325112867385, 1.000000000000000000, 0.9238795325112864054, 1.000000000000000444 ) ) 
 REPRESENTATION_ITEM ( '' )  );
#3143 = ORIENTED_EDGE ( 'NONE', *, *, #6741, .F. ) ;
#3144 = UNCERTAINTY_MEASURE_WITH_UNIT (LENGTH_MEASURE( 1.000000000000000082E-05 ), #2061, 'distance_accuracy_value', 'NONE');
#3145 = CARTESIAN_POINT ( 'NONE',  ( 10.19839929293505953, 2.406249999044085541, -24.62111388750000174 ) ) ;
#3146 = AXIS2_PLACEMENT_3D ( 'NONE', #1664, #6636, #6477 ) ;
#3147 = VECTOR ( 'NONE', #8578, 1000.000000000000000 ) ;
#3148 = EDGE_CURVE ( 'NONE', #9311, #416, #7119, .T. ) ;
#3149 = ORIENTED_EDGE ( 'NONE', *, *, #1144, .F. ) ;
#3150 = LINE ( 'NONE', #7257, #3027 ) ;
#3151 = DIRECTION ( 'NONE',  ( -0.8660254037844402619, -0.4999999999999971134, 0.000000000000000000 ) ) ;
#3152 = CARTESIAN_POINT ( 'NONE',  ( 10.19839929293505953, 1.406249999044084653, -24.62111388750000174 ) ) ;
#3153 = CARTESIAN_POINT ( 'NONE',  ( -17.67766952966369232, 3.625000000000000000, 17.67766952966368876 ) ) ;
#3154 = VECTOR ( 'NONE', #6023, 1000.000000000000000 ) ;
#3155 = CIRCLE ( 'NONE', #7238, 5.000000000000000000 ) ;
#3156 = EDGE_LOOP ( 'NONE', ( #1300, #10687, #8946, #10428 ) ) ;
#3157 = VERTEX_POINT ( 'NONE', #7029 ) ;
#3158 = CYLINDRICAL_SURFACE ( 'NONE', #8497, 25.00000000000000000 ) ;
#3159 = CARTESIAN_POINT ( 'NONE',  ( 1.285879139104720831E-15, 28.00000000000000000, 10.50000000000000000 ) ) ;
#3160 = FACE_OUTER_BOUND ( 'NONE', #1685, .T. ) ;
#3161 = CIRCLE ( 'NONE', #3891, 2.999999999999997335 ) ;
#3162 = AXIS2_PLACEMENT_3D ( 'NONE', #6257, #5422, #283 ) ;
#3163 = FACE_BOUND ( 'NONE', #8399, .T. ) ;
#3164 = DIRECTION ( 'NONE',  ( 4.710179996720586888E-17, 0.9230769230769232392, -0.3846153846153844702 ) ) ;
#3165 = ORIENTED_EDGE ( 'NONE', *, *, #6990, .T. ) ;
#3166 = ORIENTED_EDGE ( 'NONE', *, *, #4102, .T. ) ;
#3167 = AXIS2_PLACEMENT_3D ( 'NONE', #3094, #8142, #5309 ) ;
#3168 = DIRECTION ( 'NONE',  ( 0.000000000000000000, 0.000000000000000000, -1.000000000000000000 ) ) ;
#3169 = AXIS2_PLACEMENT_3D ( 'NONE', #8755, #9353, #6883 ) ;
#3170 = CARTESIAN_POINT ( 'NONE',  ( -10.19839929293507375, 4.081249999044084475, 24.62111388749999108 ) ) ;
#3171 = LINE ( 'NONE', #6568, #2815 ) ;
#3172 = CARTESIAN_POINT ( 'NONE',  ( 0.000000000000000000, 0.000000000000000000, 0.000000000000000000 ) ) ;
#3173 = CARTESIAN_POINT ( 'NONE',  ( 0.000000000000000000, 1.000000000000001998, 0.5773502691896277295 ) ) ;
#3174 = ORIENTED_EDGE ( 'NONE', *, *, #318, .T. ) ;
#3175 = DIRECTION ( 'NONE',  ( 0.000000000000000000, 0.000000000000000000, -1.000000000000000000 ) ) ;
#3176 = EDGE_CURVE ( 'NONE', #9464, #3515, #2802, .T. ) ;
#3177 = ORIENTED_EDGE ( 'NONE', *, *, #5396, .F. ) ;
#3178 = VECTOR ( 'NONE', #3137, 1000.000000000000000 ) ;
#3179 = VECTOR ( 'NONE', #890, 1000.000000000000114 ) ;
#3180 = ADVANCED_FACE ( 'NONE', ( #8011 ), #4502, .T. ) ;
#3181 = CARTESIAN_POINT ( 'NONE',  ( 24.99999999999999289, 3.549999998088169573, 10.35533905932739529 ) ) ;
#3182 = CARTESIAN_POINT ( 'NONE',  ( 17.40975659021752620, 5.093749999044084653, 17.40975659021753330 ) ) ;
#3183 = CARTESIAN_POINT ( 'NONE',  ( 24.62111388749999463, 5.331249999044085364, 10.19839929293507730 ) ) ;
#3184 = ORIENTED_EDGE ( 'NONE', *, *, #1345, .T. ) ;
#3185 = FACE_OUTER_BOUND ( 'NONE', #6312, .T. ) ;
#3186 =( NAMED_UNIT ( * ) PLANE_ANGLE_UNIT ( ) SI_UNIT ( $, .RADIAN. ) );
#3187 = AXIS2_PLACEMENT_3D ( 'NONE', #9638, #8803, #5492 ) ;
#3188 = CARTESIAN_POINT ( 'NONE',  ( 0.000000000000000000, 85.00000000000000000, 0.000000000000000000 ) ) ;
#3189 = CARTESIAN_POINT ( 'NONE',  ( 82.32050807568876394, 102.2820323027551410, 0.000000000000000000 ) ) ;
#3190 = LINE ( 'NONE', #3421, #9162 ) ;
#3191 = EDGE_CURVE ( 'NONE', #2700, #6001, #440, .T. ) ;
#3192 = CIRCLE ( 'NONE', #8864, 7.400000000000007461 ) ;
#3193 = ORIENTED_EDGE ( 'NONE', *, *, #3399, .F. ) ;
#3194 = ORIENTED_EDGE ( 'NONE', *, *, #1096, .T. ) ;
#3195 = ORIENTED_EDGE ( 'NONE', *, *, #7269, .F. ) ;
#3196 = EDGE_LOOP ( 'NONE', ( #678, #8307, #2680, #1613 ) ) ;
#3197 = AXIS2_PLACEMENT_3D ( 'NONE', #7115, #1808, #2730 ) ;
#3198 = AXIS2_PLACEMENT_3D ( 'NONE', #6243, #10483, #4588 ) ;
#3199 = EDGE_CURVE ( 'NONE', #9935, #9550, #1223, .T. ) ;
#3200 = AXIS2_PLACEMENT_3D ( 'NONE', #7516, #8563, #1011 ) ;
#3201 = DIRECTION ( 'NONE',  ( 0.000000000000000000, 0.000000000000000000, -1.000000000000000000 ) ) ;
#3202 = CARTESIAN_POINT ( 'NONE',  ( -18.60400172474257730, -0.001000000000001000089, 7.276923788646904256 ) ) ;
#3203 = VECTOR ( 'NONE', #7335, 1000.000000000000114 ) ;
#3204 = CARTESIAN_POINT ( 'NONE',  ( 0.5000000000000000000, 10.00000000000000355, -12.19615242270663202 ) ) ;
#3205 = VECTOR ( 'NONE', #3499, 1000.000000000000227 ) ;
#3206 = CARTESIAN_POINT ( 'NONE',  ( 10.19839929293505953, 2.406249999044085541, -24.62111388750000174 ) ) ;
#3207 = DIRECTION ( 'NONE',  ( 0.8660254037844380415, 0.000000000000000000, 0.5000000000000009992 ) ) ;
#3208 = AXIS2_PLACEMENT_3D ( 'NONE', #6134, #8047, #481 ) ;
#3209 = VERTEX_POINT ( 'NONE', #7909 ) ;
#3210 = VECTOR ( 'NONE', #8594, 1000.000000000000000 ) ;
#3211 = ADVANCED_FACE ( 'NONE', ( #5524 ), #8889, .T. ) ;
#3212 = EDGE_LOOP ( 'NONE', ( #9099, #5431, #77, #1769 ) ) ;
#3213 = AXIS2_PLACEMENT_3D ( 'NONE', #546, #8113, #4870 ) ;
#3214 = CARTESIAN_POINT ( 'NONE',  ( 0.000000000000000000, -1.000000000000003331, 0.5773502691896272854 ) ) ;
#3215 = TOROIDAL_SURFACE ( 'NONE', #1840, 7.399999999999999467, 0.1000000000000000472 ) ;
#3216 = DIRECTION ( 'NONE',  ( 0.000000000000000000, -1.000000000000000000, 0.000000000000000000 ) ) ;
#3217 = CARTESIAN_POINT ( 'NONE',  ( 0.000000000000000000, -0.5289809421253948152, 0.000000000000000000 ) ) ;
#3218 = CARTESIAN_POINT ( 'NONE',  ( 2.999999999999997335, 25.00000000000000000, -15.75000000000000355 ) ) ;
#3219 = LINE ( 'NONE', #644, #9579 ) ;
#3220 = EDGE_CURVE ( 'NONE', #10062, #7303, #7406, .T. ) ;
#3221 = ORIENTED_EDGE ( 'NONE', *, *, #4369, .T. ) ;
#3222 = SURFACE_SIDE_STYLE ('',( #10822 ) ) ;
#3223 = CARTESIAN_POINT ( 'NONE',  ( -10.31217782649100556, 10.00000000000000355, -6.531088913245662653 ) ) ;
#3224 = CARTESIAN_POINT ( 'NONE',  ( 1.507608415688466075E-15, 0.6437499990440845865, -24.62111388750000174 ) ) ;
#3225 = VERTEX_POINT ( 'NONE', #2048 ) ;
#3226 = DIRECTION ( 'NONE',  ( 0.000000000000000000, 0.000000000000000000, 1.000000000000000000 ) ) ;
#3227 = DIRECTION ( 'NONE',  ( -0.000000000000000000, -1.000000000000000000, -0.000000000000000000 ) ) ;
#3228 = DIRECTION ( 'NONE',  ( -2.168404344971010594E-16, 0.000000000000000000, -1.000000000000000000 ) ) ;
#3229 = LINE ( 'NONE', #773, #1544 ) ;
#3230 = VERTEX_POINT ( 'NONE', #10545 ) ;
#3231 = EDGE_LOOP ( 'NONE', ( #2528, #2669 ) ) ;
#3232 = CARTESIAN_POINT ( 'NONE',  ( 10.35533905932738286, 5.424999998088169129, 24.99999999999999645 ) ) ;
#3233 = DIRECTION ( 'NONE',  ( 1.000000000000000000, 0.000000000000000000, 0.000000000000000000 ) ) ;
#3234 = CARTESIAN_POINT ( 'NONE',  ( 24.62111388750000174, 2.281249999044085541, -10.19839929293505776 ) ) ;
#3235 = DIRECTION ( 'NONE',  ( 0.000000000000000000, 0.000000000000000000, 1.000000000000000000 ) ) ;
#3236 = ORIENTED_EDGE ( 'NONE', *, *, #6458, .F. ) ;
#3237 = CARTESIAN_POINT ( 'NONE',  ( 2.500000000000000444, -1.000000000000003109, -0.5773502691896260641 ) ) ;
#3238 = DIRECTION ( 'NONE',  ( 0.000000000000000000, 0.000000000000000000, -1.000000000000000000 ) ) ;
#3239 = DIRECTION ( 'NONE',  ( -0.2499999999999979738, 0.8660254037844380415, -0.4330127018922216853 ) ) ;
#3240 = CARTESIAN_POINT ( 'NONE',  ( 1.399999999999998579, -2.053912595556539452E-16, -7.400000000000007461 ) ) ;
#3241 = FACE_OUTER_BOUND ( 'NONE', #1800, .T. ) ;
#3242 = DIRECTION ( 'NONE',  ( 0.4999999999999887312, 0.000000000000000000, -0.8660254037844451469 ) ) ;
#3243 = ORIENTED_EDGE ( 'NONE', *, *, #6543, .F. ) ;
#3244 = ORIENTED_EDGE ( 'NONE', *, *, #8832, .T. ) ;
#3245 = ORIENTED_EDGE ( 'NONE', *, *, #4138, .T. ) ;
#3246 = ORIENTED_EDGE ( 'NONE', *, *, #7494, .F. ) ;
#3247 = EDGE_CURVE ( 'NONE', #7302, #6283, #9549, .T. ) ;
#3248 = EDGE_CURVE ( 'NONE', #1367, #2572, #6195, .T. ) ;
#3249 = CARTESIAN_POINT ( 'NONE',  ( -17.40975659021753330, 1.018749999044084698, 17.40975659021752975 ) ) ;
#3250 = CARTESIAN_POINT ( 'NONE',  ( -24.62111388750000884, 0.7812499990440845421, 10.19839929293505421 ) ) ;
#3251 = EDGE_CURVE ( 'NONE', #7713, #4798, #4069, .T. ) ;
#3252 = FACE_BOUND ( 'NONE', #6459, .T. ) ;
#3253 = VERTEX_POINT ( 'NONE', #5320 ) ;
#3254 = FACE_OUTER_BOUND ( 'NONE', #632, .T. ) ;
#3255 = FACE_OUTER_BOUND ( 'NONE', #4356, .T. ) ;
#3256 = FACE_OUTER_BOUND ( 'NONE', #2496, .T. ) ;
#3257 = CARTESIAN_POINT ( 'NONE',  ( -17.40975659021753330, 2.843749999044085097, 17.40975659021752975 ) ) ;
#3258 = CARTESIAN_POINT ( 'NONE',  ( -3.223142256880076948E-15, 28.00000000000000000, -12.75000000000000178 ) ) ;
#3259 = ADVANCED_FACE ( 'NONE', ( #1119 ), #7084, .F. ) ;
#3260 = ORIENTED_EDGE ( 'NONE', *, *, #10223, .F. ) ;
#3261 = ORIENTED_EDGE ( 'NONE', *, *, #5039, .T. ) ;
#3262 = ORIENTED_EDGE ( 'NONE', *, *, #7588, .F. ) ;
#3263 = APPLICATION_CONTEXT ( 'automotive_design' ) ;
#3264 = EDGE_LOOP ( 'NONE', ( #7982, #5182, #366, #3243 ) ) ;
#3265 = ADVANCED_FACE ( 'NONE', ( #4604 ), #9665, .T. ) ;
#3266 = DIRECTION ( 'NONE',  ( 0.000000000000000000, -1.000000000000000000, 0.000000000000000000 ) ) ;
#3267 = CARTESIAN_POINT ( 'NONE',  ( -6.531088913245624461, 10.00000000000000355, 10.31217782649102332 ) ) ;
#3268 = CARTESIAN_POINT ( 'NONE',  ( 1.399999999999998579, 1.111629890924696344E-15, 7.400000000000007461 ) ) ;
#3269 =( BOUNDED_CURVE ( )  B_SPLINE_CURVE ( 2, ( #764, #6911, #10265, #2683, #8429 ),
 .UNSPECIFIED., .F., .F. ) 
 B_SPLINE_CURVE_WITH_KNOTS ( ( 3, 2, 3 ),
 ( 0.8500000000000000888, 0.8750000000000000000, 0.8776439810613864134 ),
 .UNSPECIFIED. ) 
 CURVE ( )  GEOMETRIC_REPRESENTATION_ITEM ( )  RATIONAL_B_SPLINE_CURVE ( ( 0.9999999999999996669, 0.9238795325112870716, 1.000000000000000000, 0.9919495570230385528, 0.9856019315474255915 ) ) 
 REPRESENTATION_ITEM ( '' )  );
#3270 = CARTESIAN_POINT ( 'NONE',  ( 10.35533905932738286, 3.812500000000000000, 24.99999999999999645 ) ) ;
#3271 = CARTESIAN_POINT ( 'NONE',  ( 6.281342968951019401, 5.000000000000000888, 23.83348803927349024 ) ) ;
#3272 = ADVANCED_FACE ( 'NONE', ( #8781 ), #9617, .F. ) ;
#3273 = EDGE_LOOP ( 'NONE', ( #4492, #8232, #635, #233 ) ) ;
#3274 = CARTESIAN_POINT ( 'NONE',  ( 17.67766952966368521, 4.875000000000000000, 17.67766952966369232 ) ) ;
#3275 = DIRECTION ( 'NONE',  ( 1.000000000000000000, 0.000000000000000000, 0.000000000000000000 ) ) ;
#3276 = DIRECTION ( 'NONE',  ( 0.000000000000000000, 0.000000000000000000, 1.000000000000000000 ) ) ;
#3277 = DIRECTION ( 'NONE',  ( 0.000000000000000000, 1.000000000000000000, 0.000000000000000000 ) ) ;
#3278 = ORIENTED_EDGE ( 'NONE', *, *, #5211, .T. ) ;
#3279 = DIRECTION ( 'NONE',  ( 0.000000000000000000, 1.000000000000000000, -0.000000000000000000 ) ) ;
#3280 = DIRECTION ( 'NONE',  ( 0.000000000000000000, 1.000000000000000000, 0.000000000000000000 ) ) ;
#3281 = CARTESIAN_POINT ( 'NONE',  ( -6.982120021884462346, 10.00000000000000355, -0.5000000000000731637 ) ) ;
#3282 = EDGE_CURVE ( 'NONE', #8620, #4640, #6540, .T. ) ;
#3283 = ORIENTED_EDGE ( 'NONE', *, *, #5539, .F. ) ;
#3284 = LINE ( 'NONE', #3123, #6761 ) ;
#3285 = CARTESIAN_POINT ( 'NONE',  ( -17.40975659021752975, 2.593749999044084653, -17.40975659021752975 ) ) ;
#3286 = CLOSED_SHELL ( 'NONE', ( #9644, #10839, #279, #1210, #7602, #7468, #7615, #3180, #10654, #7942, #3743, #2261, #4847, #9466 ) ) ;
#3287 = EDGE_LOOP ( 'NONE', ( #10439, #7426, #7483, #6618 ) ) ;
#3288 = ORIENTED_EDGE ( 'NONE', *, *, #7488, .F. ) ;
#3289 = CARTESIAN_POINT ( 'NONE',  ( 24.62111388750000174, 4.393749999044084475, 0.000000000000000000 ) ) ;
#3290 = CARTESIAN_POINT ( 'NONE',  ( 0.000000000000000000, 85.00000000000000000, 0.000000000000000000 ) ) ;
#3291 = VECTOR ( 'NONE', #10406, 1000.000000000000000 ) ;
#3292 = CARTESIAN_POINT ( 'NONE',  ( -10.19839929293507552, 2.906249999044085541, 24.62111388749999463 ) ) ;
#3293 = LINE ( 'NONE', #4152, #224 ) ;
#3294 = VERTEX_POINT ( 'NONE', #3590 ) ;
#3295 = CARTESIAN_POINT ( 'NONE',  ( 0.000000000000000000, 0.000000000000000000, 5.000000000000000000 ) ) ;
#3296 =( NAMED_UNIT ( * ) PLANE_ANGLE_UNIT ( ) SI_UNIT ( $, .RADIAN. ) );
#3297 = LINE ( 'NONE', #10895, #6250 ) ;
#3298 = CARTESIAN_POINT ( 'NONE',  ( -6.982120021884474781, 10.00000000000000355, 0.4999999999999269473 ) ) ;
#3299 = DIRECTION ( 'NONE',  ( 1.000000000000000000, 0.000000000000000000, 0.000000000000000000 ) ) ;
#3300 = DIRECTION ( 'NONE',  ( -2.168404344971010347E-16, 0.000000000000000000, -1.000000000000000000 ) ) ;
#3301 = AXIS2_PLACEMENT_3D ( 'NONE', #3188, #5752, #7568 ) ;
#3302 = ORIENTED_EDGE ( 'NONE', *, *, #2465, .F. ) ;
#3303 = VERTEX_POINT ( 'NONE', #6979 ) ;
#3304 = VERTEX_POINT ( 'NONE', #2749 ) ;
#3305 = CARTESIAN_POINT ( 'NONE',  ( 10.19839929293505953, 0.5812499990440844755, -24.62111388750000174 ) ) ;
#3306 = FACE_OUTER_BOUND ( 'NONE', #4013, .T. ) ;
#3307 = CARTESIAN_POINT ( 'NONE',  ( 68.37372805638788975, 92.28203230275514102, 5.000000000000000000 ) ) ;
#3308 = VECTOR ( 'NONE', #2819, 1000.000000000000000 ) ;
#3309 = ORIENTED_EDGE ( 'NONE', *, *, #7016, .F. ) ;
#3310 = CARTESIAN_POINT ( 'NONE',  ( -6.389531198409865276, 5.000000000000000000, 23.88578866465264383 ) ) ;
#3311 = DIRECTION ( 'NONE',  ( -1.000000000000000000, 0.000000000000000000, 0.000000000000000000 ) ) ;
#3312 = CARTESIAN_POINT ( 'NONE',  ( 10.19839929293505953, 3.406249999044085097, -24.62111388750000174 ) ) ;
#3313 = CARTESIAN_POINT ( 'NONE',  ( 0.000000000000000000, 5.000000000000000000, 0.000000000000000000 ) ) ;
#3314 = CARTESIAN_POINT ( 'NONE',  ( -17.67766952966369232, 3.625000000000000000, 17.67766952966368876 ) ) ;
#3315 = ORIENTED_EDGE ( 'NONE', *, *, #5786, .T. ) ;
#3316 = EDGE_LOOP ( 'NONE', ( #1612, #10159, #3174, #6497 ) ) ;
#3317 = EDGE_CURVE ( 'NONE', #1227, #4798, #6142, .T. ) ;
#3318 = ORIENTED_EDGE ( 'NONE', *, *, #9879, .T. ) ;
#3319 = ORIENTED_EDGE ( 'NONE', *, *, #10452, .T. ) ;
#3320 = EDGE_CURVE ( 'NONE', #9769, #4894, #649, .T. ) ;
#3321 = ORIENTED_EDGE ( 'NONE', *, *, #6800, .F. ) ;
#3322 = VECTOR ( 'NONE', #5981, 1000.000000000000000 ) ;
#3323 = EDGE_CURVE ( 'NONE', #1232, #8979, #8934, .T. ) ;
#3324 = DIRECTION ( 'NONE',  ( 0.000000000000000000, 0.000000000000000000, 1.000000000000000000 ) ) ;
#3325 = DIRECTION ( 'NONE',  ( 0.000000000000000000, 0.000000000000000000, -1.000000000000000000 ) ) ;
#3326 = DIRECTION ( 'NONE',  ( 0.000000000000000000, -1.000000000000000000, 0.000000000000000000 ) ) ;
#3327 = LINE ( 'NONE', #5076, #7126 ) ;
#3328 = CARTESIAN_POINT ( 'NONE',  ( -12.19615242270663913, 10.00000000000000355, -0.5000000000001277867 ) ) ;
#3329 = CIRCLE ( 'NONE', #7580, 2.149999999999999911 ) ;
#3330 = AXIS2_PLACEMENT_3D ( 'NONE', #2859, #2905, #8834 ) ;
#3331 = EDGE_CURVE ( 'NONE', #9311, #1064, #8988, .T. ) ;
#3332 = ORIENTED_EDGE ( 'NONE', *, *, #10506, .T. ) ;
#3333 = EDGE_CURVE ( 'NONE', #8063, #10373, #3861, .T. ) ;
#3334 = CONICAL_SURFACE ( 'NONE', #9173, 22.18092213764227694, 0.3490658503988666728 ) ;
#3335 = CARTESIAN_POINT ( 'NONE',  ( 13.47724133595216500, 7.781088913245554295, -0.4999999999999529821 ) ) ;
#3336 = CARTESIAN_POINT ( 'NONE',  ( -25.00000000000001066, 4.174999998088169129, 10.35533905932737397 ) ) ;
#3337 = AXIS2_PLACEMENT_3D ( 'NONE', #3290, #1382, #4824 ) ;
#3338 =( BOUNDED_CURVE ( )  B_SPLINE_CURVE ( 3, ( #1563, #2338, #8409, #10911 ),
 .UNSPECIFIED., .F., .F. ) 
 B_SPLINE_CURVE_WITH_KNOTS ( ( 4, 4 ),
 ( 2.284520705739656155, 2.356010155625177127 ),
 .UNSPECIFIED. ) 
 CURVE ( )  GEOMETRIC_REPRESENTATION_ITEM ( )  RATIONAL_B_SPLINE_CURVE ( ( 1.000000000000000000, 0.9995741502243209453, 0.9995741502243209453, 1.000000000000000000 ) ) 
 REPRESENTATION_ITEM ( '' )  );
#3339 = VERTEX_POINT ( 'NONE', #9866 ) ;
#3340 = MANIFOLD_SOLID_BREP ( 'Cavity1', #322 ) ;
#3341 = LINE ( 'NONE', #5907, #2629 ) ;
#3342 = DIRECTION ( 'NONE',  ( 1.000000000000000000, 0.000000000000000000, 0.000000000000000000 ) ) ;
#3343 = FACE_OUTER_BOUND ( 'NONE', #1792, .T. ) ;
#3344 = CARTESIAN_POINT ( 'NONE',  ( -10.35533905932741128, 4.924999998088170905, -24.99999999999996803 ) ) ;
#3345 = CIRCLE ( 'NONE', #5, 2.999999999999997335 ) ;
#3346 = EDGE_LOOP ( 'NONE', ( #5619, #6354, #8668 ) ) ;
#3347 = COLOUR_RGB ( '', 0.66274510, 0.83137255, 0.94901961) ;
#3348 = EDGE_CURVE ( 'NONE', #4862, #9084, #701, .T. ) ;
#3349 = CARTESIAN_POINT ( 'NONE',  ( 17.40975659021752975, 2.518749999044084475, -17.40975659021752975 ) ) ;
#3350 = CARTESIAN_POINT ( 'NONE',  ( 25.52691073765301510, 98.96446609406727646, -5.000000000000000000 ) ) ;
#3351 = CARTESIAN_POINT ( 'NONE',  ( 10.19839929293505953, 4.406249999044084653, -24.62111388750000174 ) ) ;
#3352 = CYLINDRICAL_SURFACE ( 'NONE', #2852, 28.00000000000000000 ) ;
#3353 = ORIENTED_EDGE ( 'NONE', *, *, #9892, .T. ) ;
#3354 = DIRECTION ( 'NONE',  ( -0.5000000000000012212, 0.000000000000000000, -0.8660254037844380415 ) ) ;
#3355 = DIRECTION ( 'NONE',  ( 0.000000000000000000, 1.000000000000000000, 0.000000000000000000 ) ) ;
#3356 = CARTESIAN_POINT ( 'NONE',  ( -7.875000000000116351, 25.00000000000000000, -10.63990010960484334 ) ) ;
#3357 = FACE_OUTER_BOUND ( 'NONE', #6154, .T. ) ;
#3358 = DIRECTION ( 'NONE',  ( -0.000000000000000000, 1.000000000000000000, -0.000000000000000000 ) ) ;
#3359 = VECTOR ( 'NONE', #3900, 1000.000000000000000 ) ;
#3360 = MANIFOLD_SOLID_BREP ( 'Boss-Extrude2', #5953 ) ;
#3361 = ORIENTED_EDGE ( 'NONE', *, *, #6141, .T. ) ;
#3362 = EDGE_LOOP ( 'NONE', ( #8190, #2276, #9559, #580 ) ) ;
#3363 = ORIENTED_EDGE ( 'NONE', *, *, #10874, .T. ) ;
#3364 = VERTEX_POINT ( 'NONE', #489 ) ;
#3365 = UNCERTAINTY_MEASURE_WITH_UNIT (LENGTH_MEASURE( 1.000000000000000082E-05 ), #6276, 'distance_accuracy_value', 'NONE');
#3366 = CYLINDRICAL_SURFACE ( 'NONE', #7208, 25.00000000000000000 ) ;
#3367 = CARTESIAN_POINT ( 'NONE',  ( -17.40975659021752975, 0.5937499990440846531, -17.40975659021752975 ) ) ;
#3368 = AXIS2_PLACEMENT_3D ( 'NONE', #7177, #4383, #4599 ) ;
#3369 = CARTESIAN_POINT ( 'NONE',  ( -12.47307621135311351, 28.00000000000000000, 15.60400172474282599 ) ) ;
#3370 = CARTESIAN_POINT ( 'NONE',  ( -19.74999999999996803, -0.001000000000001000089, 3.000000000000206057 ) ) ;
#3371 = TOROIDAL_SURFACE ( 'NONE', #7112, 6.250000000000000000, 0.7500000000000000000 ) ;
#3372 = DIRECTION ( 'NONE',  ( 0.5000000000000012212, 0.000000000000000000, 0.8660254037844380415 ) ) ;
#3373 = DIRECTION ( 'NONE',  ( 0.000000000000000000, 0.000000000000000000, 1.000000000000000000 ) ) ;
#3374 = PLANE ( 'NONE',  #5190 ) ;
#3375 = AXIS2_PLACEMENT_3D ( 'NONE', #10383, #2797, #4801 ) ;
#3376 = VERTEX_POINT ( 'NONE', #8106 ) ;
#3377 = VECTOR ( 'NONE', #1812, 999.9999999999998863 ) ;
#3378 = VERTEX_POINT ( 'NONE', #10658 ) ;
#3379 = ORIENTED_EDGE ( 'NONE', *, *, #8473, .T. ) ;
#3380 = AXIS2_PLACEMENT_3D ( 'NONE', #1313, #2133, #4697 ) ;
#3381 = LINE ( 'NONE', #2665, #486 ) ;
#3382 = CIRCLE ( 'NONE', #1457, 2.999999999999998668 ) ;
#3383 = AXIS2_PLACEMENT_3D ( 'NONE', #7422, #10018, #10803 ) ;
#3384 = DIRECTION ( 'NONE',  ( 0.000000000000000000, -2.775557561562888270E-17, -1.000000000000000000 ) ) ;
#3385 = EDGE_CURVE ( 'NONE', #9320, #7146, #6460, .T. ) ;
#3386 = CARTESIAN_POINT ( 'NONE',  ( -4.592425496802574367E-15, 1.750000000000000000, 25.00000000000000000 ) ) ;
#3387 = CYLINDRICAL_SURFACE ( 'NONE', #6238, 2.999999999999997335 ) ;
#3388 = FACE_OUTER_BOUND ( 'NONE', #9334, .T. ) ;
#3389 = DIRECTION ( 'NONE',  ( 0.1767766952966340899, 0.3535533905932753407, 0.9185586535436918165 ) ) ;
#3390 = AXIS2_PLACEMENT_3D ( 'NONE', #786, #7684, #1667 ) ;
#3391 = AXIS2_PLACEMENT_3D ( 'NONE', #2044, #4598, #3748 ) ;
#3392 = EDGE_CURVE ( 'NONE', #3734, #5443, #3977, .T. ) ;
#3393 = CIRCLE ( 'NONE', #953, 2.999999999999997335 ) ;
#3394 = ORIENTED_EDGE ( 'NONE', *, *, #5056, .F. ) ;
#3395 = AXIS2_PLACEMENT_3D ( 'NONE', #5897, #1691, #5073 ) ;
#3396 = CARTESIAN_POINT ( 'NONE',  ( 3.933012701892183660, 10.00000000000000355, 5.812177826491091714 ) ) ;
#3397 = CARTESIAN_POINT ( 'NONE',  ( 7.875000000000019540, -0.001000000000001000089, 13.63990010960489840 ) ) ;
#3398 = CARTESIAN_POINT ( 'NONE',  ( 1.530808498934191521E-15, 3.862499998088169573, -25.00000000000000000 ) ) ;
#3399 = EDGE_CURVE ( 'NONE', #6044, #241, #5330, .T. ) ;
#3400 = DIRECTION ( 'NONE',  ( -0.000000000000000000, 1.000000000000000000, -0.000000000000000000 ) ) ;
#3401 = EDGE_LOOP ( 'NONE', ( #3024, #1755, #1813, #7534, #1740, #9802 ) ) ;
#3402 = ADVANCED_FACE ( 'NONE', ( #9376, #6675 ), #5136, .F. ) ;
#3403 = LINE ( 'NONE', #941, #7781 ) ;
#3404 = EDGE_CURVE ( 'NONE', #915, #20, #10035, .T. ) ;
#3405 = AXIS2_PLACEMENT_3D ( 'NONE', #3802, #7175, #10538 ) ;
#3406 = DIRECTION ( 'NONE',  ( -0.000000000000000000, 1.000000000000000000, -0.000000000000000000 ) ) ;
#3407 = LINE ( 'NONE', #2693, #2776 ) ;
#3408 = ADVANCED_FACE ( 'NONE', ( #821 ), #6019, .F. ) ;
#3409 = ORIENTED_EDGE ( 'NONE', *, *, #4385, .T. ) ;
#3410 = CARTESIAN_POINT ( 'NONE',  ( -4.522825247065398226E-15, 1.143749999044084475, 24.62111388750000174 ) ) ;
#3411 = CARTESIAN_POINT ( 'NONE',  ( 1.507608415688466075E-15, 2.643749999044084920, -24.62111388750000174 ) ) ;
#3412 = DIRECTION ( 'NONE',  ( 0.000000000000000000, 0.000000000000000000, 1.000000000000000000 ) ) ;
#3413 = CARTESIAN_POINT ( 'NONE',  ( 6.982120021884469452, 19.03096903053430466, -0.4999999999999756306 ) ) ;
#3414 = CYLINDRICAL_SURFACE ( 'NONE', #7265, 5.000000000000000000 ) ;
#3415 = EDGE_LOOP ( 'NONE', ( #7848, #2537, #5153, #2829 ) ) ;
#3416 = ADVANCED_FACE ( 'NONE', ( #1819 ), #872, .T. ) ;
#3417 = FACE_OUTER_BOUND ( 'NONE', #4288, .T. ) ;
#3418 = PLANE ( 'NONE',  #9594 ) ;
#3419 = CARTESIAN_POINT ( 'NONE',  ( 1.530808498934191521E-15, 0.8624999980881691286, -25.00000000000000000 ) ) ;
#3420 = CARTESIAN_POINT ( 'NONE',  ( 13.63990010960487353, -0.001000000000001000089, -7.875000000000067502 ) ) ;
#3421 = CARTESIAN_POINT ( 'NONE',  ( 0.000000000000000000, 5.000000000000000000, -25.00000000000000000 ) ) ;
#3422 = EDGE_CURVE ( 'NONE', #6438, #6764, #7551, .T. ) ;
#3423 = EDGE_LOOP ( 'NONE', ( #294, #438, #1799, #4005, #2966, #501 ) ) ;
#3424 = ORIENTED_EDGE ( 'NONE', *, *, #9145, .F. ) ;
#3425 = ORIENTED_EDGE ( 'NONE', *, *, #5954, .T. ) ;
#3426 = CARTESIAN_POINT ( 'NONE',  ( 2.999999999999999112, -0.001000000000001000089, 19.75000000000000000 ) ) ;
#3427 = CARTESIAN_POINT ( 'NONE',  ( -4.522825247065398226E-15, 0.9687499990440845421, 24.62111388750000174 ) ) ;
#3428 = DIRECTION ( 'NONE',  ( 0.000000000000000000, 1.000000000000000000, 0.000000000000000000 ) ) ;
#3429 = CARTESIAN_POINT ( 'NONE',  ( 25.00000000000000000, 5.612499998088169129, 0.000000000000000000 ) ) ;
#3430 = CARTESIAN_POINT ( 'NONE',  ( -4.522825247065398226E-15, 3.968749999044084209, 24.62111388750000174 ) ) ;
#3431 = DIRECTION ( 'NONE',  ( 0.000000000000000000, 0.000000000000000000, 1.000000000000000000 ) ) ;
#3432 = ORIENTED_EDGE ( 'NONE', *, *, #5735, .F. ) ;
#3433 = CARTESIAN_POINT ( 'NONE',  ( -10.35533905932739174, 2.299999998088169129, 24.99999999999999289 ) ) ;
#3434 = DIRECTION ( 'NONE',  ( -0.5000000000000005551, 0.8660254037844383745, 0.000000000000000000 ) ) ;
#3435 = EDGE_CURVE ( 'NONE', #10325, #6438, #992, .T. ) ;
#3436 = CARTESIAN_POINT ( 'NONE',  ( -4.592425496802574367E-15, 0.7500000000000000000, 25.00000000000000000 ) ) ;
#3437 = DIRECTION ( 'NONE',  ( 0.000000000000000000, -9.470910429910653047E-17, 1.000000000000000000 ) ) ;
#3438 = ORIENTED_EDGE ( 'NONE', *, *, #5204, .T. ) ;
#3439 = ORIENTED_EDGE ( 'NONE', *, *, #727, .F. ) ;
#3440 = ORIENTED_EDGE ( 'NONE', *, *, #3323, .F. ) ;
#3441 = ORIENTED_EDGE ( 'NONE', *, *, #1609, .T. ) ;
#3442 = DIRECTION ( 'NONE',  ( 0.000000000000000000, -1.000000000000000000, 0.000000000000000000 ) ) ;
#3443 = CARTESIAN_POINT ( 'NONE',  ( -17.10400172474275848, 28.00000000000000000, -9.874999999999836575 ) ) ;
#3444 = ORIENTED_EDGE ( 'NONE', *, *, #2281, .T. ) ;
#3445 = FACE_OUTER_BOUND ( 'NONE', #8136, .T. ) ;
#3446 = CARTESIAN_POINT ( 'NONE',  ( 10.47307621135333200, 28.00000000000000000, 12.13990010960489840 ) ) ;
#3447 = LINE ( 'NONE', #2731, #3772 ) ;
#3448 = CARTESIAN_POINT ( 'NONE',  ( 0.000000000000000000, 20.00000000000000355, 0.000000000000000000 ) ) ;
#3449 = CARTESIAN_POINT ( 'NONE',  ( 11.42163336986827815, 7.781088913245564953, 7.171633369868360752 ) ) ;
#3450 = ORIENTED_EDGE ( 'NONE', *, *, #6211, .F. ) ;
#3451 = PRODUCT_DEFINITION ( 'UNKNOWN', '', #6353, #7052 ) ;
#3452 = ORIENTED_EDGE ( 'NONE', *, *, #7252, .T. ) ;
#3453 = DIRECTION ( 'NONE',  ( 1.000000000000000000, 0.000000000000000000, 0.000000000000000000 ) ) ;
#3454 = DIRECTION ( 'NONE',  ( 0.5000000000000009992, -0.8660254037844380415, 1.745740669421570228E-15 ) ) ;
#3455 = CARTESIAN_POINT ( 'NONE',  ( 25.00000000000000000, 5.612499998088169129, 0.000000000000000000 ) ) ;
#3456 = CARTESIAN_POINT ( 'NONE',  ( 18.60400172474268032, 25.00000000000000000, 7.276923788646641356 ) ) ;
#3457 = MANIFOLD_SOLID_BREP ( 'Boss-Extrude3', #10008 ) ;
#3458 = DIRECTION ( 'NONE',  ( -0.8660254037844434816, 0.000000000000000000, -0.4999999999999918399 ) ) ;
#3459 = LINE ( 'NONE', #3281, #3948 ) ;
#3460 = FACE_OUTER_BOUND ( 'NONE', #1167, .T. ) ;
#3461 = LINE ( 'NONE', #10102, #3109 ) ;
#3462 = MECHANICAL_DESIGN_GEOMETRIC_PRESENTATION_REPRESENTATION (  '', ( #9483 ), #7711 ) ;
#3463 = EDGE_CURVE ( 'NONE', #2038, #6538, #3269, .T. ) ;
#3464 = EDGE_CURVE ( 'NONE', #3339, #6001, #6083, .T. ) ;
#3465 = CARTESIAN_POINT ( 'NONE',  ( 24.62111388750000174, 0.3937499990440845865, 0.000000000000000000 ) ) ;
#3466 = CARTESIAN_POINT ( 'NONE',  ( -17.40975659021752975, 2.768749999044084475, -17.40975659021752975 ) ) ;
#3467 = DIRECTION ( 'NONE',  ( -1.000000000000000000, 0.000000000000000000, 3.708321773340234242E-15 ) ) ;
#3468 = CARTESIAN_POINT ( 'NONE',  ( 24.62111388750000174, 4.281249999044084653, -10.19839929293505776 ) ) ;
#3469 = DIRECTION ( 'NONE',  ( 0.000000000000000000, -0.000000000000000000, 1.000000000000000000 ) ) ;
#3470 = ORIENTED_EDGE ( 'NONE', *, *, #2649, .T. ) ;
#3471 = CARTESIAN_POINT ( 'NONE',  ( -19.74999999999996803, 28.00000000000000000, 3.000000000000206057 ) ) ;
#3472 = ADVANCED_FACE ( 'NONE', ( #36 ), #8320, .F. ) ;
#3473 = CARTESIAN_POINT ( 'NONE',  ( 0.000000000000000000, 88.00000000000001421, 0.000000000000000000 ) ) ;
#3474 = VECTOR ( 'NONE', #7931, 1000.000000000000000 ) ;
#3475 = CARTESIAN_POINT ( 'NONE',  ( 6.305607966083884186, 7.781088913245563177, -11.92163336986830480 ) ) ;
#3476 = CARTESIAN_POINT ( 'NONE',  ( -25.00000000000001421, 2.174999998088169573, 10.35533905932737397 ) ) ;
#3477 = CARTESIAN_POINT ( 'NONE',  ( 66.68467533811312364, 89.45240317130979690, 5.000000000000000000 ) ) ;
#3478 = CARTESIAN_POINT ( 'NONE',  ( -10.35533905932737575, 4.312500000000000888, -25.00000000000000000 ) ) ;
#3479 = VECTOR ( 'NONE', #8259, 1000.000000000000000 ) ;
#3480 = ORIENTED_EDGE ( 'NONE', *, *, #508, .F. ) ;
#3481 = EDGE_CURVE ( 'NONE', #7721, #9883, #9878, .T. ) ;
#3482 = ORIENTED_EDGE ( 'NONE', *, *, #10855, .T. ) ;
#3483 = ORIENTED_EDGE ( 'NONE', *, *, #5251, .F. ) ;
#3484 = CIRCLE ( 'NONE', #3851, 2.999999999999996891 ) ;
#3485 = DIRECTION ( 'NONE',  ( 0.000000000000000000, 1.000000000000000000, 0.000000000000000000 ) ) ;
#3486 = CARTESIAN_POINT ( 'NONE',  ( 24.62111388750000174, 0.2812499990440845976, -10.19839929293505776 ) ) ;
#3487 = DIRECTION ( 'NONE',  ( -0.000000000000000000, -0.000000000000000000, 1.000000000000000000 ) ) ;
#3488 = CARTESIAN_POINT ( 'NONE',  ( -24.62111388750000174, 2.893749999044084475, -3.015216831376932151E-15 ) ) ;
#3489 = CARTESIAN_POINT ( 'NONE',  ( -10.19839929293505776, 3.531249999044084653, -24.62111388750000174 ) ) ;
#3490 = DIRECTION ( 'NONE',  ( 0.000000000000000000, 1.000000000000000000, -0.000000000000000000 ) ) ;
#3491 = EDGE_CURVE ( 'NONE', #883, #8678, #7592, .T. ) ;
#3492 = ORIENTED_EDGE ( 'NONE', *, *, #1270, .T. ) ;
#3493 = CARTESIAN_POINT ( 'NONE',  ( 2.999999999999996447, 25.00000000000000000, -19.75000000000000000 ) ) ;
#3494 = FACE_OUTER_BOUND ( 'NONE', #750, .T. ) ;
#3495 = CARTESIAN_POINT ( 'NONE',  ( -0.5000000000000000000, 0.000000000000000000, 0.000000000000000000 ) ) ;
#3496 = CARTESIAN_POINT ( 'NONE',  ( 0.000000000000000000, 7.000000000000003553, 0.000000000000000000 ) ) ;
#3497 = VECTOR ( 'NONE', #5808, 1000.000000000000000 ) ;
#3498 = CARTESIAN_POINT ( 'NONE',  ( 10.35533905932737930, 1.187500000000000444, -25.00000000000000000 ) ) ;
#3499 = DIRECTION ( 'NONE',  ( 0.1889822365046257002, -0.000000000000000000, -0.9819805060619632986 ) ) ;
#3500 = ORIENTED_EDGE ( 'NONE', *, *, #6344, .T. ) ;
#3501 = VERTEX_POINT ( 'NONE', #4421 ) ;
#3502 = ORIENTED_EDGE ( 'NONE', *, *, #4369, .F. ) ;
#3503 = ORIENTED_EDGE ( 'NONE', *, *, #3247, .F. ) ;
#3504 = PLANE ( 'NONE',  #5612 ) ;
#3505 = EDGE_CURVE ( 'NONE', #8502, #7190, #8039, .T. ) ;
#3506 = DIRECTION ( 'NONE',  ( 1.000000000000000000, 0.000000000000000000, 0.000000000000000000 ) ) ;
#3507 = CARTESIAN_POINT ( 'NONE',  ( 24.99999999999999289, 1.937500000000000000, 10.35533905932739529 ) ) ;
#3508 = DIRECTION ( 'NONE',  ( 0.000000000000000000, -2.775557561562888270E-17, -1.000000000000000000 ) ) ;
#3509 = CARTESIAN_POINT ( 'NONE',  ( -15.13990010960496235, 25.00000000000000000, -5.276923788646544544 ) ) ;
#3510 = CARTESIAN_POINT ( 'NONE',  ( 0.000000000000000000, 0.000000000000000000, 0.000000000000000000 ) ) ;
#3511 = PLANE ( 'NONE',  #566 ) ;
#3512 = CARTESIAN_POINT ( 'NONE',  ( -1.500000000000001332, -1.595945597898662527E-16, -5.750000000000006217 ) ) ;
#3513 = EDGE_LOOP ( 'NONE', ( #900, #2101, #9843, #1391 ) ) ;
#3514 = PRODUCT_DEFINITION_FORMATION_WITH_SPECIFIED_SOURCE ( 'ANY', '', #4613, .NOT_KNOWN. ) ;
#3515 = VERTEX_POINT ( 'NONE', #3578 ) ;
#3516 = CARTESIAN_POINT ( 'NONE',  ( -17.10400172474254532, 25.00000000000000000, 9.875000000000202505 ) ) ;
#3517 = CARTESIAN_POINT ( 'NONE',  ( -25.00000000000000000, 4.112499998088169129, -3.061616997868383043E-15 ) ) ;
#3518 = CARTESIAN_POINT ( 'NONE',  ( 24.62111388750000174, 2.456249999044084475, -10.19839929293505776 ) ) ;
#3519 = CARTESIAN_POINT ( 'NONE',  ( -6.145599950363554775, 19.66631150450992038, -3.355508642977555578 ) ) ;
#3520 = CARTESIAN_POINT ( 'NONE',  ( -11.06217782649100734, 10.00000000000000355, -6.386751345948264103 ) ) ;
#3521 = CIRCLE ( 'NONE', #10432, 5.000000000000000000 ) ;
#3522 = CIRCLE ( 'NONE', #10411, 27.91176187412962761 ) ;
#3523 = CARTESIAN_POINT ( 'NONE',  ( 5.796693311223918066, 19.03096903053432598, -3.924072712834439702 ) ) ;
#3524 = PLANE ( 'NONE',  #5279 ) ;
#3525 = AXIS2_PLACEMENT_3D ( 'NONE', #6846, #9445, #10268 ) ;
#3526 = AXIS2_PLACEMENT_3D ( 'NONE', #3629, #8720, #1163 ) ;
#3527 = CARTESIAN_POINT ( 'NONE',  ( -24.62111388750000174, 2.831249999044084475, -10.19839929293506131 ) ) ;
#3528 = CARTESIAN_POINT ( 'NONE',  ( 0.000000000000000000, -58.00000000000000000, 0.000000000000000000 ) ) ;
#3529 = DIRECTION ( 'NONE',  ( 1.000000000000000000, 0.000000000000000000, 0.000000000000000000 ) ) ;
#3530 = CARTESIAN_POINT ( 'NONE',  ( 3.061616997868383043E-15, 82.00000000000000000, -25.00000000000000000 ) ) ;
#3531 = EDGE_LOOP ( 'NONE', ( #9699, #10736 ) ) ;
#3532 = CARTESIAN_POINT ( 'NONE',  ( -25.00000000000000000, 1.112499998088169351, -3.061616997868383043E-15 ) ) ;
#3533 = CARTESIAN_POINT ( 'NONE',  ( 10.35533905932738286, 1.424999998088169129, 24.99999999999999645 ) ) ;
#3534 = CARTESIAN_POINT ( 'NONE',  ( 1.507608415688466075E-15, 0.4687499990440845421, -24.62111388750000174 ) ) ;
#3535 = EDGE_CURVE ( 'NONE', #795, #4001, #1990, .T. ) ;
#3536 = CARTESIAN_POINT ( 'NONE',  ( -4.592425496802574367E-15, 2.362499998088169129, 25.00000000000000000 ) ) ;
#3537 = DIRECTION ( 'NONE',  ( 0.000000000000000000, 1.000000000000000000, 0.000000000000000000 ) ) ;
#3538 = VECTOR ( 'NONE', #1185, 1000.000000000000114 ) ;
#3539 = EDGE_CURVE ( 'NONE', #10806, #5726, #4245, .T. ) ;
#3540 = ORIENTED_EDGE ( 'NONE', *, *, #8344, .F. ) ;
#3541 = ORIENTED_EDGE ( 'NONE', *, *, #10104, .T. ) ;
#3542 = ADVANCED_FACE ( 'NONE', ( #1304 ), #899, .T. ) ;
#3543 = FACE_OUTER_BOUND ( 'NONE', #10485, .T. ) ;
#3544 = CARTESIAN_POINT ( 'NONE',  ( -17.40975659021753330, 3.018749999044084475, 17.40975659021752975 ) ) ;
#3545 = CARTESIAN_POINT ( 'NONE',  ( 17.40975659021752975, 0.5187499990440846975, -17.40975659021752975 ) ) ;
#3546 = CARTESIAN_POINT ( 'NONE',  ( -25.00000000000000000, 5.112499998088170017, -3.061616997868383043E-15 ) ) ;
#3547 = CARTESIAN_POINT ( 'NONE',  ( 10.19839929293506486, 4.031249999044083765, 24.62111388749999819 ) ) ;
#3548 = PLANE ( 'NONE',  #7547 ) ;
#3549 = AXIS2_PLACEMENT_3D ( 'NONE', #5110, #6714, #7420 ) ;
#3550 = ADVANCED_FACE ( 'NONE', ( #4688 ), #2297, .T. ) ;
#3551 = CARTESIAN_POINT ( 'NONE',  ( 2.500000000000000444, 1.000000000000001998, 0.5773502691896277295 ) ) ;
#3552 = EDGE_CURVE ( 'NONE', #5695, #7304, #5138, .T. ) ;
#3553 = DIRECTION ( 'NONE',  ( 0.000000000000000000, 1.000000000000000000, 0.000000000000000000 ) ) ;
#3554 = CARTESIAN_POINT ( 'NONE',  ( 67.97877056362573001, 89.28203230275514102, -5.000000000000000000 ) ) ;
#3555 = CARTESIAN_POINT ( 'NONE',  ( -25.00000000000001421, 0.5625000000000001110, 10.35533905932737397 ) ) ;
#3556 = CARTESIAN_POINT ( 'NONE',  ( 27.32050807568876749, 100.0000000000000142, 5.000000000000000000 ) ) ;
#3557 = ORIENTED_EDGE ( 'NONE', *, *, #738, .T. ) ;
#3558 = ORIENTED_EDGE ( 'NONE', *, *, #9439, .T. ) ;
#3559 = EDGE_LOOP ( 'NONE', ( #6413, #7496, #8083 ) ) ;
#3560 = EDGE_LOOP ( 'NONE', ( #8976, #5605, #7607, #4686 ) ) ;
#3561 = EDGE_CURVE ( 'NONE', #2252, #7275, #1748, .T. ) ;
#3562 = DIRECTION ( 'NONE',  ( 1.000000000000000000, 0.000000000000000000, 0.000000000000000000 ) ) ;
#3563 = AXIS2_PLACEMENT_3D ( 'NONE', #7962, #5424, #167 ) ;
#3564 = DIRECTION ( 'NONE',  ( 0.000000000000000000, 1.000000000000000000, 0.000000000000000000 ) ) ;
#3565 = ORIENTED_EDGE ( 'NONE', *, *, #9583, .F. ) ;
#3566 = CARTESIAN_POINT ( 'NONE',  ( 82.32050807568876394, 92.28203230275514102, 0.000000000000000000 ) ) ;
#3567 = CARTESIAN_POINT ( 'NONE',  ( -6.386751345948222358, 10.00000000000000355, 11.06217782649103221 ) ) ;
#3568 = AXIS2_PLACEMENT_3D ( 'NONE', #2036, #1984, #3628 ) ;
#3569 = CARTESIAN_POINT ( 'NONE',  ( 3.223142256880076948E-15, 25.00000000000000000, 15.75000000000000000 ) ) ;
#3570 = LINE ( 'NONE', #8718, #7591 ) ;
#3571 = CYLINDRICAL_SURFACE ( 'NONE', #10462, 25.00000000000000000 ) ;
#3572 = CARTESIAN_POINT ( 'NONE',  ( -17.40975659021753330, 5.018749999044084475, 17.40975659021752975 ) ) ;
#3573 = EDGE_CURVE ( 'NONE', #3052, #7535, #8086, .T. ) ;
#3574 = EDGE_LOOP ( 'NONE', ( #9908, #2349, #8533, #9673, #2490, #5984 ) ) ;
#3575 = AXIS2_PLACEMENT_3D ( 'NONE', #2309, #9985, #2413 ) ;
#3576 = ADVANCED_FACE ( 'NONE', ( #6441 ), #7849, .F. ) ;
#3577 = VERTEX_POINT ( 'NONE', #3955 ) ;
#3578 = CARTESIAN_POINT ( 'NONE',  ( 1.399999999999998579, 1.126651916477731646E-15, 7.500000000000000000 ) ) ;
#3579 = CARTESIAN_POINT ( 'NONE',  ( -25.00000000000000000, 4.500000000000000888, -3.061616997868383043E-15 ) ) ;
#3580 = CARTESIAN_POINT ( 'NONE',  ( 1.507608415688466075E-15, 3.643749999044084920, -24.62111388750000174 ) ) ;
#3581 = FACE_OUTER_BOUND ( 'NONE', #7448, .T. ) ;
#3582 = CONTEXT_DEPENDENT_SHAPE_REPRESENTATION ( #6682, #272 ) ;
#3583 = AXIS2_PLACEMENT_3D ( 'NONE', #314, #3626, #1160 ) ;
#3584 = FACE_OUTER_BOUND ( 'NONE', #10661, .T. ) ;
#3585 = LINE ( 'NONE', #1936, #5517 ) ;
#3586 = FACE_OUTER_BOUND ( 'NONE', #8888, .T. ) ;
#3587 = EDGE_CURVE ( 'NONE', #3515, #7146, #9700, .T. ) ;
#3588 = AXIS2_PLACEMENT_3D ( 'NONE', #10317, #9648, #4477 ) ;
#3589 = CARTESIAN_POINT ( 'NONE',  ( 0.000000000000000000, 20.00000000000000355, 0.000000000000000000 ) ) ;
#3590 = CARTESIAN_POINT ( 'NONE',  ( 5.276923788646705304, 25.00000000000000000, 15.13990010960490196 ) ) ;
#3591 = CIRCLE ( 'NONE', #10653, 22.00000000000000355 ) ;
#3592 = CARTESIAN_POINT ( 'NONE',  ( 1.530808498934191521E-15, 0.8624999980881691286, -25.00000000000000000 ) ) ;
#3593 = LINE ( 'NONE', #6145, #561 ) ;
#3594 = EDGE_LOOP ( 'NONE', ( #4590, #6969, #6282, #8093 ) ) ;
#3595 = FACE_OUTER_BOUND ( 'NONE', #9895, .T. ) ;
#3596 = CARTESIAN_POINT ( 'NONE',  ( -25.00000000000001066, 2.562500000000000444, 10.35533905932737397 ) ) ;
#3597 = LINE ( 'NONE', #8622, #8326 ) ;
#3598 = DIRECTION ( 'NONE',  ( -0.8660254037844431485, 0.000000000000000000, -0.4999999999999922839 ) ) ;
#3599 = CARTESIAN_POINT ( 'NONE',  ( 10.35533905932738286, 2.812500000000000000, 24.99999999999999645 ) ) ;
#3600 = ORIENTED_EDGE ( 'NONE', *, *, #4315, .F. ) ;
#3601 = ORIENTED_EDGE ( 'NONE', *, *, #10945, .F. ) ;
#3602 = ORIENTED_EDGE ( 'NONE', *, *, #10048, .T. ) ;
#3603 = FACE_OUTER_BOUND ( 'NONE', #7170, .T. ) ;
#3604 = CARTESIAN_POINT ( 'NONE',  ( 10.19839929293506486, 5.206249999044084475, 24.62111388749999819 ) ) ;
#3605 = CARTESIAN_POINT ( 'NONE',  ( -19.74999999999996803, 28.00000000000000000, 3.000000000000206057 ) ) ;
#3606 = CARTESIAN_POINT ( 'NONE',  ( 1.530808498934191521E-15, 4.862499998088169129, -25.00000000000000000 ) ) ;
#3607 = CARTESIAN_POINT ( 'NONE',  ( -10.19839929293507552, 2.906249999044085541, 24.62111388749999463 ) ) ;
#3608 = DIRECTION ( 'NONE',  ( -1.000000000000000000, 0.000000000000000000, 0.000000000000000000 ) ) ;
#3609 = FACE_OUTER_BOUND ( 'NONE', #538, .T. ) ;
#3610 = PLANE ( 'NONE',  #5678 ) ;
#3611 = DIRECTION ( 'NONE',  ( -0.000000000000000000, 1.000000000000000000, -0.000000000000000000 ) ) ;
#3612 = CYLINDRICAL_SURFACE ( 'NONE', #10472, 25.00000000000000000 ) ;
#3613 = EDGE_LOOP ( 'NONE', ( #6889, #1348 ) ) ;
#3614 = VERTEX_POINT ( 'NONE', #9744 ) ;
#3615 = ORIENTED_EDGE ( 'NONE', *, *, #10700, .F. ) ;
#3616 = EDGE_CURVE ( 'NONE', #241, #8189, #7254, .T. ) ;
#3617 = ORIENTED_EDGE ( 'NONE', *, *, #7890, .F. ) ;
#3618 = EDGE_CURVE ( 'NONE', #6230, #7276, #4254, .T. ) ;
#3619 = LINE ( 'NONE', #8648, #7036 ) ;
#3620 = ADVANCED_FACE ( 'NONE', ( #8602 ), #7786, .F. ) ;
#3621 = LINE ( 'NONE', #4346, #5871 ) ;
#3622 = ORIENTED_EDGE ( 'NONE', *, *, #7467, .F. ) ;
#3623 = CARTESIAN_POINT ( 'NONE',  ( 0.000000000000000000, 31.00000000000000000, -10.50000000000000000 ) ) ;
#3624 = EDGE_CURVE ( 'NONE', #10065, #5382, #7449, .T. ) ;
#3625 = CARTESIAN_POINT ( 'NONE',  ( 17.10400172474269098, 25.00000000000000000, 9.874999999999957367 ) ) ;
#3626 = DIRECTION ( 'NONE',  ( -0.000000000000000000, -1.000000000000000000, -0.000000000000000000 ) ) ;
#3627 = DIRECTION ( 'NONE',  ( -0.000000000000000000, -1.000000000000000000, -0.000000000000000000 ) ) ;
#3628 = DIRECTION ( 'NONE',  ( -0.8660254037844328234, 0.000000000000000000, -0.5000000000000101030 ) ) ;
#3629 = CARTESIAN_POINT ( 'NONE',  ( 0.000000000000000000, 0.000000000000000000, 0.000000000000000000 ) ) ;
#3630 = ORIENTED_EDGE ( 'NONE', *, *, #2138, .F. ) ;
#3631 = ORIENTED_EDGE ( 'NONE', *, *, #8540, .F. ) ;
#3632 = EDGE_CURVE ( 'NONE', #3304, #5761, #6709, .T. ) ;
#3633 = ORIENTED_EDGE ( 'NONE', *, *, #4017, .F. ) ;
#3634 = EDGE_CURVE ( 'NONE', #8678, #883, #2624, .T. ) ;
#3635 = CARTESIAN_POINT ( 'NONE',  ( 25.00000000000000000, 3.000000000000000000, 0.000000000000000000 ) ) ;
#3636 = DIRECTION ( 'NONE',  ( -3.491481338843133355E-15, 0.000000000000000000, 1.000000000000000000 ) ) ;
#3637 = CARTESIAN_POINT ( 'NONE',  ( -17.40975659021753330, 2.018749999044084475, 17.40975659021752975 ) ) ;
#3638 = VERTEX_POINT ( 'NONE', #3369 ) ;
#3639 = LINE ( 'NONE', #5311, #4956 ) ;
#3640 = ADVANCED_FACE ( 'NONE', ( #3306 ), #2435, .T. ) ;
#3641 = DIRECTION ( 'NONE',  ( 0.000000000000000000, -1.000000000000000000, 0.000000000000000000 ) ) ;
#3642 = CARTESIAN_POINT ( 'NONE',  ( 0.000000000000000000, 10.00000000000000355, 0.000000000000000000 ) ) ;
#3643 = DIRECTION ( 'NONE',  ( -0.000000000000000000, -1.000000000000000000, -0.000000000000000000 ) ) ;
#3644 = DIRECTION ( 'NONE',  ( 0.000000000000000000, 1.000000000000000000, 0.000000000000000000 ) ) ;
#3645 = EDGE_CURVE ( 'NONE', #2130, #514, #3521, .T. ) ;
#3646 = CARTESIAN_POINT ( 'NONE',  ( 10.35533905932737930, 2.187500000000000444, -25.00000000000000000 ) ) ;
#3647 = DIRECTION ( 'NONE',  ( 0.000000000000000000, 0.000000000000000000, -1.000000000000000000 ) ) ;
#3648 = CARTESIAN_POINT ( 'NONE',  ( -17.40975659021752975, 0.7687499990440845865, -17.40975659021752975 ) ) ;
#3649 = ORIENTED_EDGE ( 'NONE', *, *, #1464, .F. ) ;
#3650 = CARTESIAN_POINT ( 'NONE',  ( -0.2499999999999960032, 0.000000000000000000, -0.4330127018922216298 ) ) ;
#3651 =( LENGTH_UNIT ( ) NAMED_UNIT ( * ) SI_UNIT ( .MILLI., .METRE. ) );
#3652 = CARTESIAN_POINT ( 'NONE',  ( -10.35533905932737575, 2.312500000000000888, -25.00000000000000000 ) ) ;
#3653 = FACE_OUTER_BOUND ( 'NONE', #4025, .T. ) ;
#3654 = CARTESIAN_POINT ( 'NONE',  ( 0.000000000000000000, 8.000000000000000000, 0.000000000000000000 ) ) ;
#3655 =( BOUNDED_CURVE ( )  B_SPLINE_CURVE ( 2, ( #2298, #10872, #8159, #3971, #3106 ),
 .UNSPECIFIED., .F., .F. ) 
 B_SPLINE_CURVE_WITH_KNOTS ( ( 3, 2, 3 ),
 ( 0.000000000000000000, 0.02500000000000000486, 0.05000000000000000971 ),
 .UNSPECIFIED. ) 
 CURVE ( )  GEOMETRIC_REPRESENTATION_ITEM ( )  RATIONAL_B_SPLINE_CURVE ( ( 1.000000000000000000, 0.9238795325112867385, 1.000000000000000000, 0.9238795325112867385, 1.000000000000000000 ) ) 
 REPRESENTATION_ITEM ( '' )  );
#3656 = ORIENTED_EDGE ( 'NONE', *, *, #8257, .T. ) ;
#3657 = EDGE_LOOP ( 'NONE', ( #8206, #6387, #3244, #10682 ) ) ;
#3658 = CARTESIAN_POINT ( 'NONE',  ( -17.40975659021753330, 2.018749999044084475, 17.40975659021752975 ) ) ;
#3659 = ORIENTED_EDGE ( 'NONE', *, *, #10086, .F. ) ;
#3660 = MECHANICAL_DESIGN_GEOMETRIC_PRESENTATION_REPRESENTATION (  '', ( #7351 ), #310 ) ;
#3661 = CARTESIAN_POINT ( 'NONE',  ( 10.19839929293506486, 4.031249999044083765, 24.62111388749999819 ) ) ;
#3662 = CARTESIAN_POINT ( 'NONE',  ( 0.5590169943749494497, 0.000000000000000000, 0.000000000000000000 ) ) ;
#3663 = CARTESIAN_POINT ( 'NONE',  ( 1.530808498934191521E-15, 2.862499998088169573, -25.00000000000000000 ) ) ;
#3664 = CARTESIAN_POINT ( 'NONE',  ( -17.67766952966368876, 0.3750000000000000000, -17.67766952966369232 ) ) ;
#3665 =( LENGTH_UNIT ( ) NAMED_UNIT ( * ) SI_UNIT ( .MILLI., .METRE. ) );
#3666 = CARTESIAN_POINT ( 'NONE',  ( 3.058047309050022200, 19.03096903053434019, -6.296693311223905631 ) ) ;
#3667 = FACE_OUTER_BOUND ( 'NONE', #3156, .T. ) ;
#3668 = DIRECTION ( 'NONE',  ( 0.000000000000000000, 0.000000000000000000, 1.000000000000000000 ) ) ;
#3669 = DIRECTION ( 'NONE',  ( -0.000000000000000000, -0.000000000000000000, 1.000000000000000000 ) ) ;
#3670 = PRESENTATION_LAYER_ASSIGNMENT (  '', '', ( #10192 ) ) ;
#3671 = DIRECTION ( 'NONE',  ( -0.000000000000000000, -1.000000000000000000, -0.000000000000000000 ) ) ;
#3672 = ORIENTED_EDGE ( 'NONE', *, *, #5396, .T. ) ;
#3673 = AXIS2_PLACEMENT_3D ( 'NONE', #1200, #7985, #7111 ) ;
#3674 = ORIENTED_EDGE ( 'NONE', *, *, #10458, .F. ) ;
#3675 = ORIENTED_EDGE ( 'NONE', *, *, #2201, .T. ) ;
#3676 = VERTEX_POINT ( 'NONE', #1454 ) ;
#3677 = FACE_OUTER_BOUND ( 'NONE', #6607, .T. ) ;
#3678 = COLOUR_RGB ( '', 0.66274510, 0.83137255, 0.94901961) ;
#3679 = AXIS2_PLACEMENT_3D ( 'NONE', #6756, #4205, #1550 ) ;
#3680 = DIRECTION ( 'NONE',  ( -0.4999999999999917288, 0.000000000000000000, 0.8660254037844434816 ) ) ;
#3681 = DIRECTION ( 'NONE',  ( -0.000000000000000000, 1.000000000000000000, -0.000000000000000000 ) ) ;
#3682 = DIRECTION ( 'NONE',  ( -0.000000000000000000, -1.000000000000000000, -0.000000000000000000 ) ) ;
#3683 = DIRECTION ( 'NONE',  ( 0.000000000000000000, -0.000000000000000000, 1.000000000000000000 ) ) ;
#3684 = ADVANCED_FACE ( 'NONE', ( #5815 ), #7393, .F. ) ;
#3685 = CARTESIAN_POINT ( 'NONE',  ( 1.500000000000001332, 0.000000000000000000, 0.000000000000000000 ) ) ;
#3686 = CARTESIAN_POINT ( 'NONE',  ( -10.31217782649113524, 10.00000000000000355, 6.531088913245442384 ) ) ;
#3687 = PLANE ( 'NONE',  #5319 ) ;
#3688 = VECTOR ( 'NONE', #6792, 1000.000000000000227 ) ;
#3689 = ADVANCED_FACE ( 'NONE', ( #9900 ), #9284, .F. ) ;
#3690 = ORIENTED_EDGE ( 'NONE', *, *, #8287, .T. ) ;
#3691 = SURFACE_STYLE_USAGE ( .BOTH. , #7901 ) ;
#3692 = CARTESIAN_POINT ( 'NONE',  ( 24.62111388750000174, 3.456249999044084920, -10.19839929293505776 ) ) ;
#3693 = DIRECTION ( 'NONE',  ( 0.4999999999999947820, 0.000000000000000000, -0.8660254037844417052 ) ) ;
#3694 = DIRECTION ( 'NONE',  ( 0.000000000000000000, 0.000000000000000000, 1.000000000000000000 ) ) ;
#3695 = FACE_OUTER_BOUND ( 'NONE', #7178, .T. ) ;
#3696 = EDGE_CURVE ( 'NONE', #5553, #2787, #8816, .T. ) ;
#3697 = ORIENTED_EDGE ( 'NONE', *, *, #7106, .F. ) ;
#3698 = ORIENTED_EDGE ( 'NONE', *, *, #3003, .T. ) ;
#3699 = VERTEX_POINT ( 'NONE', #1294 ) ;
#3700 = EDGE_CURVE ( 'NONE', #2407, #6845, #9067, .T. ) ;
#3701 = AXIS2_PLACEMENT_3D ( 'NONE', #5044, #3940, #4828 ) ;
#3702 = CARTESIAN_POINT ( 'NONE',  ( -17.40975659021753330, 5.018749999044084475, 17.40975659021752975 ) ) ;
#3703 = CARTESIAN_POINT ( 'NONE',  ( 15.75000000000000000, 28.00000000000000000, -5.821397334365942453E-14 ) ) ;
#3704 = CARTESIAN_POINT ( 'NONE',  ( -22.42673455797375937, 5.000000000000000000, 10.41080002251884018 ) ) ;
#3705 = VECTOR ( 'NONE', #9949, 1000.000000000000000 ) ;
#3706 = CARTESIAN_POINT ( 'NONE',  ( 3.061616997868383043E-15, 5.000000000000000000, 25.00000000000000000 ) ) ;
#3707 = ORIENTED_EDGE ( 'NONE', *, *, #3080, .F. ) ;
#3708 = FACE_OUTER_BOUND ( 'NONE', #9958, .T. ) ;
#3709 = SURFACE_SIDE_STYLE ('',( #3072 ) ) ;
#3710 = CARTESIAN_POINT ( 'NONE',  ( 0.000000000000000000, 7.000000000000003553, 0.000000000000000000 ) ) ;
#3711 = CARTESIAN_POINT ( 'NONE',  ( 1.507608415688466075E-15, 2.468749999044085097, -24.62111388750000174 ) ) ;
#3712 = CARTESIAN_POINT ( 'NONE',  ( 11.12916512459886675, 10.00000000000000355, -6.580127018922165227 ) ) ;
#3713 = VERTEX_POINT ( 'NONE', #3134 ) ;
#3714 = VECTOR ( 'NONE', #3865, 1000.000000000000000 ) ;
#3715 = ORIENTED_EDGE ( 'NONE', *, *, #10471, .F. ) ;
#3716 = VECTOR ( 'NONE', #2263, 1000.000000000000000 ) ;
#3717 = VERTEX_POINT ( 'NONE', #9884 ) ;
#3718 = ADVANCED_FACE ( 'NONE', ( #10674 ), #2475, .T. ) ;
#3719 = ORIENTED_EDGE ( 'NONE', *, *, #7379, .T. ) ;
#3720 = LINE ( 'NONE', #8746, #3538 ) ;
#3721 = CARTESIAN_POINT ( 'NONE',  ( 24.62111388750000174, 1.281249999044084653, -10.19839929293505776 ) ) ;
#3722 = CARTESIAN_POINT ( 'NONE',  ( -10.19839929293505776, 1.706249999044084698, -24.62111388750000174 ) ) ;
#3723 = CARTESIAN_POINT ( 'NONE',  ( -10.35533905932739174, 4.687500000000000888, 24.99999999999999289 ) ) ;
#3724 =( NAMED_UNIT ( * ) SI_UNIT ( $, .STERADIAN. ) SOLID_ANGLE_UNIT ( ) );
#3725 =( BOUNDED_CURVE ( )  B_SPLINE_CURVE ( 2, ( #6259, #7860, #1225, #5322, #3762, #285, #3648, #9668, #2751, #5381, #7032, #5266, #10498, #7139, #10392, #2094, #8738, #5470, #4375, #7739, #6925, #10282, #6095, #9455, #1887, #8619, #10660, #1483, #5526, #10705, #9927, #2305, #8109, #9869, #7227, #8013, #442, #4658, #5686, #4810, #1421, #601, #6510, #4866, #8991, #4754, #8210, #2145, #4706, #651, #4028, #543, #5579, #8936, #8169, #9719, #7381, #2199, #3979, #3170, #3069, #3809, #5632, #7182, #10760, #7329, #1325, #3115, #9053, #2361, #6565, #2956, #10547, #5739, #3921, #1370, #2246, #1276, #6361, #10602, #8054 ),
 .UNSPECIFIED., .F., .F. ) 
 B_SPLINE_CURVE_WITH_KNOTS ( ( 3, 2, 2, 2, 2, 2, 2, 2, 2, 2, 2, 2, 2, 2, 2, 2, 2, 2, 2, 2, 2, 2, 2, 2, 2, 2, 2, 2, 2, 2, 2, 2, 2, 2, 2, 2, 2, 2, 2, 2, 3 ),
 ( 0.000000000000000000, 0.02500000000000000139, 0.05000000000000000278, 0.07499999999999999722, 0.1000000000000000056, 0.1250000000000000000, 0.1499999999999999944, 0.1749999999999999889, 0.2000000000000000111, 0.2250000000000000056, 0.2500000000000000000, 0.2750000000000000222, 0.2999999999999999889, 0.3250000000000000111, 0.3499999999999999778, 0.3750000000000000000, 0.4000000000000000222, 0.4249999999999999889, 0.4500000000000000111, 0.4749999999999999778, 0.5000000000000000000, 0.5250000000000000222, 0.5500000000000000444, 0.5749999999999999556, 0.5999999999999999778, 0.6250000000000000000, 0.6500000000000000222, 0.6750000000000000444, 0.6999999999999999556, 0.7249999999999999778, 0.7500000000000000000, 0.7750000000000000222, 0.8000000000000000444, 0.8249999999999999556, 0.8499999999999999778, 0.8750000000000000000, 0.9000000000000000222, 0.9250000000000000444, 0.9499999999999999556, 0.9749999999999999778, 1.000000000000000000 ),
 .UNSPECIFIED. ) 
 CURVE ( )  GEOMETRIC_REPRESENTATION_ITEM ( )  RATIONAL_B_SPLINE_CURVE ( ( 1.000000000000000000, 0.9238795325112867385, 1.000000000000000000, 0.9238795325112867385, 1.000000000000000000, 0.9238795325112867385, 1.000000000000000000, 0.9238795325112867385, 1.000000000000000000, 0.9238795325112867385, 1.000000000000000000, 0.9238795325112867385, 1.000000000000000000, 0.9238795325112867385, 1.000000000000000000, 0.9238795325112867385, 1.000000000000000000, 0.9238795325112867385, 1.000000000000000000, 0.9238795325112867385, 1.000000000000000000, 0.9238795325112867385, 1.000000000000000000, 0.9238795325112867385, 1.000000000000000000, 0.9238795325112867385, 1.000000000000000000, 0.9238795325112867385, 1.000000000000000000, 0.9238795325112867385, 1.000000000000000000, 0.9238795325112867385, 1.000000000000000000, 0.9238795325112867385, 1.000000000000000000, 0.9238795325112867385, 1.000000000000000000, 0.9238795325112867385, 1.000000000000000000, 0.9238795325112867385, 1.000000000000000000, 0.9238795325112867385, 1.000000000000000000, 0.9238795325112867385, 1.000000000000000000, 0.9238795325112867385, 1.000000000000000000, 0.9238795325112867385, 1.000000000000000000, 0.9238795325112867385, 1.000000000000000000, 0.9238795325112867385, 1.000000000000000000, 0.9238795325112867385, 1.000000000000000000, 0.9238795325112867385, 1.000000000000000000, 0.9238795325112867385, 1.000000000000000000, 0.9238795325112867385, 1.000000000000000000, 0.9238795325112867385, 1.000000000000000000, 0.9238795325112867385, 1.000000000000000000, 0.9238795325112867385, 1.000000000000000000, 0.9238795325112867385, 1.000000000000000000, 0.9238795325112867385, 1.000000000000000000, 0.9238795325112867385, 1.000000000000000000, 0.9238795325112867385, 1.000000000000000000, 0.9238795325112867385, 1.000000000000000000, 0.9238795325112867385, 1.000000000000000000, 0.9238795325112867385, 1.000000000000000000 ) ) 
 REPRESENTATION_ITEM ( '' )  );
#3726 = CARTESIAN_POINT ( 'NONE',  ( 2.694222958124177204E-15, 5.000000000000000000, 22.00000000000000355 ) ) ;
#3727 = CARTESIAN_POINT ( 'NONE',  ( -19.75000000000000000, -0.001000000000001000089, 2.108281996628241301E-13 ) ) ;
#3728 = DIRECTION ( 'NONE',  ( 0.000000000000000000, 1.000000000000000000, 0.000000000000000000 ) ) ;
#3729 = LINE ( 'NONE', #5290, #4242 ) ;
#3730 = ORIENTED_EDGE ( 'NONE', *, *, #1584, .T. ) ;
#3731 = AXIS2_PLACEMENT_3D ( 'NONE', #4944, #5664, #5759 ) ;
#3732 = CARTESIAN_POINT ( 'NONE',  ( 3.061616997868383043E-15, 0.000000000000000000, 25.00000000000000000 ) ) ;
#3733 = DIRECTION ( 'NONE',  ( 0.000000000000000000, 1.000000000000000000, 0.000000000000000000 ) ) ;
#3734 = VERTEX_POINT ( 'NONE', #722 ) ;
#3735 = DIRECTION ( 'NONE',  ( 0.000000000000000000, 0.000000000000000000, -1.000000000000000000 ) ) ;
#3736 = DIRECTION ( 'NONE',  ( 0.000000000000000000, 0.000000000000000000, 1.000000000000000000 ) ) ;
#3737 = CARTESIAN_POINT ( 'NONE',  ( -3.208128317448845301, 19.34316356887878641, -6.223805082245781328 ) ) ;
#3738 = DIRECTION ( 'NONE',  ( -0.000000000000000000, 1.000000000000000000, -0.000000000000000000 ) ) ;
#3739 = CIRCLE ( 'NONE', #918, 2.999999999999996891 ) ;
#3740 = ORIENTED_EDGE ( 'NONE', *, *, #7323, .T. ) ;
#3741 = AXIS2_PLACEMENT_3D ( 'NONE', #7606, #3277, #10932 ) ;
#3742 = ORIENTED_EDGE ( 'NONE', *, *, #9879, .F. ) ;
#3743 = ADVANCED_FACE ( 'NONE', ( #6585 ), #8391, .T. ) ;
#3744 = AXIS2_PLACEMENT_3D ( 'NONE', #10225, #6866, #381 ) ;
#3745 = CARTESIAN_POINT ( 'NONE',  ( 24.62111388749999108, 4.331249999044084475, 10.19839929293507730 ) ) ;
#3746 = CARTESIAN_POINT ( 'NONE',  ( -3.924072712834500543, 10.00000000000000355, 5.796693311223878098 ) ) ;
#3747 = LINE ( 'NONE', #7127, #5379 ) ;
#3748 = DIRECTION ( 'NONE',  ( 0.000000000000000000, -2.775557561562887961E-17, -1.000000000000000000 ) ) ;
#3749 = DIRECTION ( 'NONE',  ( 0.000000000000000000, 0.000000000000000000, 1.000000000000000000 ) ) ;
#3750 = ADVANCED_FACE ( 'NONE', ( #8279 ), #1547, .F. ) ;
#3751 = AXIS2_PLACEMENT_3D ( 'NONE', #8765, #148, #3508 ) ;
#3752 = AXIS2_PLACEMENT_3D ( 'NONE', #9851, #5614, #7214 ) ;
#3753 = ORIENTED_EDGE ( 'NONE', *, *, #1741, .F. ) ;
#3754 = EDGE_LOOP ( 'NONE', ( #9740, #10701, #2911, #9106, #3070, #10295 ) ) ;
#3755 = EDGE_CURVE ( 'NONE', #3125, #7345, #5643, .T. ) ;
#3756 = ADVANCED_FACE ( 'NONE', ( #1498, #4931 ), #1435, .T. ) ;
#3757 = EDGE_CURVE ( 'NONE', #3230, #4608, #10227, .T. ) ;
#3758 = CIRCLE ( 'NONE', #3575, 2.999999999999999112 ) ;
#3759 = CARTESIAN_POINT ( 'NONE',  ( -24.62111388750000884, 4.956249999044084475, 10.19839929293505421 ) ) ;
#3760 = DIRECTION ( 'NONE',  ( 0.000000000000000000, 0.8660254037844387076, -0.4999999999999999445 ) ) ;
#3761 = CARTESIAN_POINT ( 'NONE',  ( 68.37372805638788975, 97.28203230275514102, 5.000000000000000000 ) ) ;
#3762 = CARTESIAN_POINT ( 'NONE',  ( 1.507608415688466075E-15, 0.6437499990440845865, -24.62111388750000174 ) ) ;
#3763 = EDGE_LOOP ( 'NONE', ( #9605, #8045 ) ) ;
#3764 = DIRECTION ( 'NONE',  ( -0.000000000000000000, 1.000000000000000000, -0.000000000000000000 ) ) ;
#3765 = FACE_OUTER_BOUND ( 'NONE', #2728, .T. ) ;
#3766 = VERTEX_POINT ( 'NONE', #9168 ) ;
#3767 = AXIS2_PLACEMENT_3D ( 'NONE', #2604, #2489, #4171 ) ;
#3768 = CARTESIAN_POINT ( 'NONE',  ( -24.62111388750000884, 4.781249999044083765, 10.19839929293505421 ) ) ;
#3769 = CARTESIAN_POINT ( 'NONE',  ( 25.00000000000000000, 2.612499998088169129, 0.000000000000000000 ) ) ;
#3770 = EDGE_CURVE ( 'NONE', #20, #10157, #5750, .T. ) ;
#3771 = TOROIDAL_SURFACE ( 'NONE', #581, 5.100000000000000533, 0.1000000000000001582 ) ;
#3772 = VECTOR ( 'NONE', #10198, 1000.000000000000000 ) ;
#3773 = ORIENTED_EDGE ( 'NONE', *, *, #8689, .F. ) ;
#3774 = VERTEX_POINT ( 'NONE', #9994 ) ;
#3775 = CIRCLE ( 'NONE', #6958, 2.999999999999999112 ) ;
#3776 = EDGE_CURVE ( 'NONE', #10524, #3818, #613, .T. ) ;
#3777 = DIRECTION ( 'NONE',  ( -0.000000000000000000, -1.000000000000000000, -0.000000000000000000 ) ) ;
#3778 = CARTESIAN_POINT ( 'NONE',  ( 24.62111388749999463, 2.156249999044085097, 10.19839929293507730 ) ) ;
#3779 = CARTESIAN_POINT ( 'NONE',  ( 17.40975659021752620, 2.268749999044084475, 17.40975659021753330 ) ) ;
#3780 = AXIS2_PLACEMENT_3D ( 'NONE', #10812, #3216, #2192 ) ;
#3781 = CARTESIAN_POINT ( 'NONE',  ( 1.530808498934191521E-15, 2.250000000000000444, -25.00000000000000000 ) ) ;
#3782 = SHAPE_REPRESENTATION_RELATIONSHIP ( 'NONE' , 'NONE' ,  #5436, #9554 ) ;
#3783 = DIRECTION ( 'NONE',  ( 0.000000000000000000, -0.8660254037844387076, 0.4999999999999999445 ) ) ;
#3784 = CARTESIAN_POINT ( 'NONE',  ( -25.00000000000000000, 1.112499998088169351, -3.061616997868383043E-15 ) ) ;
#3785 = DIRECTION ( 'NONE',  ( 0.8660254037844407060, 0.4999999999999965583, -0.000000000000000000 ) ) ;
#3786 = CARTESIAN_POINT ( 'NONE',  ( 25.00000000000000000, -2.710505431213761085E-17, 0.000000000000000000 ) ) ;
#3787 = EDGE_CURVE ( 'NONE', #7897, #399, #6690, .T. ) ;
#3788 = CIRCLE ( 'NONE', #2853, 5.000000000000000888 ) ;
#3789 = EDGE_LOOP ( 'NONE', ( #213, #1539, #4820, #4514, #8721, #7694 ) ) ;
#3790 = ORIENTED_EDGE ( 'NONE', *, *, #9500, .T. ) ;
#3791 = ORIENTED_EDGE ( 'NONE', *, *, #3404, .T. ) ;
#3792 = PLANE ( 'NONE',  #7831 ) ;
#3793 = CARTESIAN_POINT ( 'NONE',  ( 0.000000000000000000, 85.00000000000000000, 0.000000000000000000 ) ) ;
#3794 = CARTESIAN_POINT ( 'NONE',  ( 1.564302918553086774E-15, 7.000000000000003553, -12.77350269189627063 ) ) ;
#3795 = DIRECTION ( 'NONE',  ( -0.000000000000000000, 0.000000000000000000, -1.000000000000000000 ) ) ;
#3796 = DIRECTION ( 'NONE',  ( -0.000000000000000000, -1.000000000000000000, -0.000000000000000000 ) ) ;
#3797 = ORIENTED_EDGE ( 'NONE', *, *, #7898, .F. ) ;
#3798 = ORIENTED_EDGE ( 'NONE', *, *, #7234, .F. ) ;
#3799 = CARTESIAN_POINT ( 'NONE',  ( -5.237222008264700033E-15, 0.000000000000000000, 0.5000000000000000000 ) ) ;
#3800 = EDGE_CURVE ( 'NONE', #3774, #10263, #4988, .T. ) ;
#3801 = DIRECTION ( 'NONE',  ( 0.8660254037844417052, 0.000000000000000000, 0.4999999999999947820 ) ) ;
#3802 = CARTESIAN_POINT ( 'NONE',  ( 0.000000000000000000, -55.00000000000000000, 0.000000000000000000 ) ) ;
#3803 = DIRECTION ( 'NONE',  ( 0.000000000000000000, 0.000000000000000000, -1.000000000000000000 ) ) ;
#3804 = CARTESIAN_POINT ( 'NONE',  ( 0.000000000000000000, 10.00000000000000355, 0.000000000000000000 ) ) ;
#3805 = ORIENTED_EDGE ( 'NONE', *, *, #1008, .T. ) ;
#3806 = ORIENTED_EDGE ( 'NONE', *, *, #9634, .T. ) ;
#3807 = CARTESIAN_POINT ( 'NONE',  ( -1.500000000000000444, 83.00000000000000000, -1.500000000000000222 ) ) ;
#3808 = CARTESIAN_POINT ( 'NONE',  ( -23.76354281994116846, 5.000000000000000000, -7.534344838453043813 ) ) ;
#3809 = CARTESIAN_POINT ( 'NONE',  ( 10.19839929293506486, 4.206249999044083587, 24.62111388749999819 ) ) ;
#3810 = ORIENTED_EDGE ( 'NONE', *, *, #5114, .T. ) ;
#3811 = DIRECTION ( 'NONE',  ( 1.445602896647339163E-16, 0.000000000000000000, 1.000000000000000000 ) ) ;
#3812 = SURFACE_STYLE_USAGE ( .BOTH. , #3709 ) ;
#3813 = DIRECTION ( 'NONE',  ( 0.000000000000000000, -0.000000000000000000, 1.000000000000000000 ) ) ;
#3814 = ORIENTED_EDGE ( 'NONE', *, *, #4017, .T. ) ;
#3815 = CARTESIAN_POINT ( 'NONE',  ( 10.19839929293506486, 2.031249999044084653, 24.62111388749999819 ) ) ;
#3816 = DIRECTION ( 'NONE',  ( -0.000000000000000000, 1.000000000000000000, -0.000000000000000000 ) ) ;
#3817 = EDGE_CURVE ( 'NONE', #7899, #4897, #9009, .T. ) ;
#3818 = VERTEX_POINT ( 'NONE', #2266 ) ;
#3819 = ADVANCED_FACE ( 'NONE', ( #3185 ), #5650, .F. ) ;
#3820 = ORIENTED_EDGE ( 'NONE', *, *, #6894, .F. ) ;
#3821 = VERTEX_POINT ( 'NONE', #9007 ) ;
#3822 = ORIENTED_EDGE ( 'NONE', *, *, #7885, .T. ) ;
#3823 = EDGE_CURVE ( 'NONE', #9950, #9951, #4946, .T. ) ;
#3824 = CARTESIAN_POINT ( 'NONE',  ( -0.5000000000000000000, 19.03096903053430822, -6.982120021884467675 ) ) ;
#3825 = CARTESIAN_POINT ( 'NONE',  ( 17.40975659021752620, 1.093749999044084653, 17.40975659021753330 ) ) ;
#3826 = CARTESIAN_POINT ( 'NONE',  ( 24.62111388750000174, 4.456249999044085364, -10.19839929293505776 ) ) ;
#3827 = EDGE_LOOP ( 'NONE', ( #10899, #3719, #7995, #7315 ) ) ;
#3828 = CARTESIAN_POINT ( 'NONE',  ( -4.592425496802574367E-15, 1.750000000000000000, 25.00000000000000000 ) ) ;
#3829 = CARTESIAN_POINT ( 'NONE',  ( -10.00000000000000000, 93.00000000000001421, 5.000000000000000000 ) ) ;
#3830 = FACE_OUTER_BOUND ( 'NONE', #9551, .T. ) ;
#3831 = CARTESIAN_POINT ( 'NONE',  ( 0.000000000000000000, -55.00000000000000000, 27.91176187412963117 ) ) ;
#3832 = DIRECTION ( 'NONE',  ( 0.000000000000000000, -1.000000000000000000, 0.000000000000000000 ) ) ;
#3833 = EDGE_CURVE ( 'NONE', #2200, #2242, #7377, .T. ) ;
#3834 = MECHANICAL_DESIGN_GEOMETRIC_PRESENTATION_REPRESENTATION (  '', ( #8942 ), #6887 ) ;
#3835 = VERTEX_POINT ( 'NONE', #1837 ) ;
#3836 = ORIENTED_EDGE ( 'NONE', *, *, #8352, .T. ) ;
#3837 = EDGE_CURVE ( 'NONE', #3225, #7963, #7423, .T. ) ;
#3838 = CARTESIAN_POINT ( 'NONE',  ( -25.00000000000000000, 4.437500000000001776, -10.35533905932738108 ) ) ;
#3839 = VECTOR ( 'NONE', #8168, 1000.000000000000000 ) ;
#3840 = PRESENTATION_STYLE_ASSIGNMENT (( #4735 ) ) ;
#3841 = CARTESIAN_POINT ( 'NONE',  ( 14.00000000000000533, 0.000000000000000000, 0.000000000000000000 ) ) ;
#3842 = CARTESIAN_POINT ( 'NONE',  ( -15.60400172474278158, 28.00000000000000000, -12.47307621135316680 ) ) ;
#3843 = CARTESIAN_POINT ( 'NONE',  ( -1.400000000000001910, -1.387778780781445676E-16, -5.000000000000005329 ) ) ;
#3844 = LINE ( 'NONE', #5723, #7625 ) ;
#3845 = EDGE_LOOP ( 'NONE', ( #4045, #8485, #8647, #9852, #842, #967 ) ) ;
#3846 = EDGE_CURVE ( 'NONE', #963, #849, #10410, .T. ) ;
#3847 = VERTEX_POINT ( 'NONE', #6927 ) ;
#3848 = AXIS2_PLACEMENT_3D ( 'NONE', #9411, #7700, #7924 ) ;
#3849 = EDGE_CURVE ( 'NONE', #7097, #10741, #5670, .T. ) ;
#3850 = ORIENTED_EDGE ( 'NONE', *, *, #4167, .T. ) ;
#3851 = AXIS2_PLACEMENT_3D ( 'NONE', #5438, #2165, #10565 ) ;
#3852 = DIRECTION ( 'NONE',  ( 0.4999999999999949485, 0.000000000000000000, 0.8660254037844415942 ) ) ;
#3853 = DIRECTION ( 'NONE',  ( -0.000000000000000000, -1.000000000000000000, -0.000000000000000000 ) ) ;
#3854 = CARTESIAN_POINT ( 'NONE',  ( 0.5000000000000000000, 19.03096903053429756, -6.982120021884467675 ) ) ;
#3855 = DIRECTION ( 'NONE',  ( -0.000000000000000000, 1.000000000000000000, 0.000000000000000000 ) ) ;
#3856 = CARTESIAN_POINT ( 'NONE',  ( -12.47307621135311351, -0.001000000000001000089, 15.60400172474282599 ) ) ;
#3857 = APPLICATION_CONTEXT ( 'automotive_design' ) ;
#3858 = CIRCLE ( 'NONE', #1926, 2.999999999999999112 ) ;
#3859 = ORIENTED_EDGE ( 'NONE', *, *, #10780, .F. ) ;
#3860 = ORIENTED_EDGE ( 'NONE', *, *, #10607, .F. ) ;
#3861 = LINE ( 'NONE', #1481, #4793 ) ;
#3862 = FACE_OUTER_BOUND ( 'NONE', #1378, .T. ) ;
#3863 = LINE ( 'NONE', #3013, #6234 ) ;
#3864 = VERTEX_POINT ( 'NONE', #5976 ) ;
#3865 = DIRECTION ( 'NONE',  ( 1.000000000000000000, 0.000000000000000000, 0.000000000000000000 ) ) ;
#3866 =( NAMED_UNIT ( * ) PLANE_ANGLE_UNIT ( ) SI_UNIT ( $, .RADIAN. ) );
#3867 = CARTESIAN_POINT ( 'NONE',  ( 25.00000000000000000, 2.674999998088169573, -10.35533905932737753 ) ) ;
#3868 = ORIENTED_EDGE ( 'NONE', *, *, #2469, .T. ) ;
#3869 = CARTESIAN_POINT ( 'NONE',  ( 17.40975659021752975, 1.343749999044084653, -17.40975659021752975 ) ) ;
#3870 = LINE ( 'NONE', #7038, #6329 ) ;
#3871 = EDGE_LOOP ( 'NONE', ( #9480, #10454, #7966, #4729 ) ) ;
#3872 = AXIS2_PLACEMENT_3D ( 'NONE', #1586, #2364, #3280 ) ;
#3873 = LINE ( 'NONE', #9681, #3308 ) ;
#3874 = CARTESIAN_POINT ( 'NONE',  ( 10.19839929293506486, 3.031249999044084653, 24.62111388749999819 ) ) ;
#3875 = CARTESIAN_POINT ( 'NONE',  ( 17.40975659021752975, 1.518749999044084698, -17.40975659021752975 ) ) ;
#3876 = ORIENTED_EDGE ( 'NONE', *, *, #3963, .F. ) ;
#3877 = ADVANCED_FACE ( 'NONE', ( #2637 ), #4260, .T. ) ;
#3878 = CARTESIAN_POINT ( 'NONE',  ( -25.00000000000000000, 2.437500000000000444, -10.35533905932738108 ) ) ;
#3879 = CARTESIAN_POINT ( 'NONE',  ( -6.982120021884462346, 19.03096903053432243, -0.5000000000000731637 ) ) ;
#3880 = CARTESIAN_POINT ( 'NONE',  ( -17.67766952966369232, 1.237499998088169129, 17.67766952966368876 ) ) ;
#3881 = CARTESIAN_POINT ( 'NONE',  ( -10.00000000000000000, 90.00000000000001421, 0.000000000000000000 ) ) ;
#3882 = CARTESIAN_POINT ( 'NONE',  ( 3.061616997868383043E-15, 82.00000000000000000, -25.00000000000000000 ) ) ;
#3883 = AXIS2_PLACEMENT_3D ( 'NONE', #1824, #10097, #6086 ) ;
#3884 = VECTOR ( 'NONE', #6324, 1000.000000000000000 ) ;
#3885 = ADVANCED_FACE ( 'NONE', ( #1065 ), #10284, .F. ) ;
#3886 = ORIENTED_EDGE ( 'NONE', *, *, #4529, .T. ) ;
#3887 = ORIENTED_EDGE ( 'NONE', *, *, #2012, .F. ) ;
#3888 = ORIENTED_EDGE ( 'NONE', *, *, #10193, .T. ) ;
#3889 = ORIENTED_EDGE ( 'NONE', *, *, #5183, .T. ) ;
#3890 = CARTESIAN_POINT ( 'NONE',  ( 1.530808498934191521E-15, 0.2500000000000000000, -25.00000000000000000 ) ) ;
#3891 = AXIS2_PLACEMENT_3D ( 'NONE', #6127, #1750, #1983 ) ;
#3892 = AXIS2_PLACEMENT_3D ( 'NONE', #6694, #888, #831 ) ;
#3893 = EDGE_CURVE ( 'NONE', #5479, #7535, #957, .T. ) ;
#3894 = DIRECTION ( 'NONE',  ( 1.000000000000000000, 0.000000000000000000, 0.000000000000000000 ) ) ;
#3895 = EDGE_CURVE ( 'NONE', #4070, #1064, #5982, .T. ) ;
#3896 = CARTESIAN_POINT ( 'NONE',  ( 68.37372805638788975, 97.28203230275514102, -5.000000000000000000 ) ) ;
#3897 = CYLINDRICAL_SURFACE ( 'NONE', #5003, 2.999999999999997335 ) ;
#3898 = VERTEX_POINT ( 'NONE', #58 ) ;
#3899 = CYLINDRICAL_SURFACE ( 'NONE', #9046, 25.00000000000000000 ) ;
#3900 = DIRECTION ( 'NONE',  ( -0.000000000000000000, 1.000000000000000000, -0.000000000000000000 ) ) ;
#3901 = CARTESIAN_POINT ( 'NONE',  ( -3.499999999999921840, 20.00000000000000355, -6.062177826491114807 ) ) ;
#3902 = DIRECTION ( 'NONE',  ( 0.5000000000000009992, 0.000000000000000000, 0.8660254037844380415 ) ) ;
#3903 = EDGE_CURVE ( 'NONE', #6283, #3230, #5920, .T. ) ;
#3904 = AXIS2_PLACEMENT_3D ( 'NONE', #7105, #10470, #2884 ) ;
#3905 = AXIS2_PLACEMENT_3D ( 'NONE', #3112, #5684, #2511 ) ;
#3906 = ORIENTED_EDGE ( 'NONE', *, *, #7269, .T. ) ;
#3907 = ORIENTED_EDGE ( 'NONE', *, *, #8828, .T. ) ;
#3908 = EDGE_LOOP ( 'NONE', ( #3091, #1132, #7338, #10849 ) ) ;
#3909 = EDGE_CURVE ( 'NONE', #7721, #10062, #7683, .T. ) ;
#3910 = DIRECTION ( 'NONE',  ( -0.000000000000000000, -1.000000000000000000, -0.000000000000000000 ) ) ;
#3911 = CARTESIAN_POINT ( 'NONE',  ( 0.000000000000000000, -58.00000000000000000, 0.000000000000000000 ) ) ;
#3912 = DIRECTION ( 'NONE',  ( 0.000000000000000000, 1.000000000000000000, 0.000000000000000000 ) ) ;
#3913 = VECTOR ( 'NONE', #8909, 1000.000000000000000 ) ;
#3914 = ADVANCED_FACE ( 'NONE', ( #3595 ), #6983, .F. ) ;
#3915 = DIRECTION ( 'NONE',  ( 0.5000000000000009992, 0.000000000000000000, -0.8660254037844380415 ) ) ;
#3916 = ADVANCED_FACE ( 'NONE', ( #3417 ), #8503, .F. ) ;
#3917 = ORIENTED_EDGE ( 'NONE', *, *, #6870, .T. ) ;
#3918 = VERTEX_POINT ( 'NONE', #112 ) ;
#3919 = AXIS2_PLACEMENT_3D ( 'NONE', #4625, #2883, #6278 ) ;
#3920 =( LENGTH_UNIT ( ) NAMED_UNIT ( * ) SI_UNIT ( .MILLI., .METRE. ) );
#3921 = CARTESIAN_POINT ( 'NONE',  ( -17.40975659021753330, 5.018749999044084475, 17.40975659021752975 ) ) ;
#3922 = ORIENTED_EDGE ( 'NONE', *, *, #5204, .F. ) ;
#3923 = AXIS2_PLACEMENT_3D ( 'NONE', #9166, #6806, #1835 ) ;
#3924 = CARTESIAN_POINT ( 'NONE',  ( 24.81055694375000087, 5.109374999522041882, 0.000000000000000000 ) ) ;
#3925 = CARTESIAN_POINT ( 'NONE',  ( 7.875000000000019540, 25.00000000000000000, 13.63990010960489840 ) ) ;
#3926 = EDGE_CURVE ( 'NONE', #10105, #3577, #9269, .T. ) ;
#3927 = ORIENTED_EDGE ( 'NONE', *, *, #2196, .F. ) ;
#3928 = CARTESIAN_POINT ( 'NONE',  ( -24.62111388750000174, 3.656249999044084653, -10.19839929293506131 ) ) ;
#3929 = CARTESIAN_POINT ( 'NONE',  ( 10.19839929293506486, 3.031249999044084653, 24.62111388749999819 ) ) ;
#3930 = VECTOR ( 'NONE', #8719, 1000.000000000000000 ) ;
#3931 = VERTEX_POINT ( 'NONE', #444 ) ;
#3932 = ORIENTED_EDGE ( 'NONE', *, *, #1696, .T. ) ;
#3933 = AXIS2_PLACEMENT_3D ( 'NONE', #10025, #2447, #9301 ) ;
#3934 = ORIENTED_EDGE ( 'NONE', *, *, #8768, .F. ) ;
#3935 = VECTOR ( 'NONE', #5261, 1000.000000000000114 ) ;
#3936 = CARTESIAN_POINT ( 'NONE',  ( 17.67766952966369232, 3.737499998088169573, -17.67766952966369232 ) ) ;
#3937 = DIRECTION ( 'NONE',  ( 0.000000000000000000, -2.775557561562888270E-17, -1.000000000000000000 ) ) ;
#3938 = VECTOR ( 'NONE', #9906, 1000.000000000000114 ) ;
#3939 = CARTESIAN_POINT ( 'NONE',  ( 24.62111388749999463, 1.331249999044084475, 10.19839929293507730 ) ) ;
#3940 = DIRECTION ( 'NONE',  ( 0.000000000000000000, 1.000000000000000000, 0.000000000000000000 ) ) ;
#3941 = CARTESIAN_POINT ( 'NONE',  ( 0.000000000000000000, 85.00000000000000000, 0.000000000000000000 ) ) ;
#3942 = AXIS2_PLACEMENT_3D ( 'NONE', #422, #10838, #8865 ) ;
#3943 = FACE_OUTER_BOUND ( 'NONE', #428, .T. ) ;
#3944 = DIRECTION ( 'NONE',  ( -0.2499999999999949762, -0.8660254037844380415, -0.4330127018922234061 ) ) ;
#3945 = CIRCLE ( 'NONE', #5371, 2.999999999999998224 ) ;
#3946 = DIRECTION ( 'NONE',  ( 0.000000000000000000, 0.000000000000000000, -1.000000000000000000 ) ) ;
#3947 = EDGE_LOOP ( 'NONE', ( #9642, #1156 ) ) ;
#3948 = VECTOR ( 'NONE', #1763, 1000.000000000000000 ) ;
#3949 = ORIENTED_EDGE ( 'NONE', *, *, #2395, .F. ) ;
#3950 = ORIENTED_EDGE ( 'NONE', *, *, #5389, .F. ) ;
#3951 = EDGE_LOOP ( 'NONE', ( #5906, #4563 ) ) ;
#3952 = VECTOR ( 'NONE', #1864, 1000.000000000000000 ) ;
#3953 = UNCERTAINTY_MEASURE_WITH_UNIT (LENGTH_MEASURE( 1.000000000000000082E-05 ), #171, 'distance_accuracy_value', 'NONE');
#3954 = CARTESIAN_POINT ( 'NONE',  ( -4.592425496802574367E-15, 3.750000000000000000, 25.00000000000000000 ) ) ;
#3955 = CARTESIAN_POINT ( 'NONE',  ( -15.74999999999997158, 28.00000000000000000, 3.000000000000165645 ) ) ;
#3956 = AXIS2_PLACEMENT_3D ( 'NONE', #5312, #5260, #3694 ) ;
#3957 = CARTESIAN_POINT ( 'NONE',  ( 1.530808498934191521E-15, 4.862499998088169129, -25.00000000000000000 ) ) ;
#3958 = DIRECTION ( 'NONE',  ( -0.000000000000000000, -0.000000000000000000, -1.000000000000000000 ) ) ;
#3959 = CARTESIAN_POINT ( 'NONE',  ( 15.60400172474269453, 28.00000000000000000, 12.47307621135327693 ) ) ;
#3960 = DIRECTION ( 'NONE',  ( 0.000000000000000000, 1.000000000000000000, 0.000000000000000000 ) ) ;
#3961 = VERTEX_POINT ( 'NONE', #7229 ) ;
#3962 = EDGE_CURVE ( 'NONE', #1334, #857, #4661, .T. ) ;
#3963 = EDGE_CURVE ( 'NONE', #7572, #5862, #4556, .T. ) ;
#3964 = VERTEX_POINT ( 'NONE', #10394 ) ;
#3965 = VERTEX_POINT ( 'NONE', #1179 ) ;
#3966 = EDGE_LOOP ( 'NONE', ( #2040, #6861, #909 ) ) ;
#3967 = EDGE_CURVE ( 'NONE', #9358, #8587, #6261, .T. ) ;
#3968 = DIRECTION ( 'NONE',  ( 1.047444401652940007E-14, 0.000000000000000000, -1.000000000000000000 ) ) ;
#3969 = CARTESIAN_POINT ( 'NONE',  ( 1.530808498934191521E-15, 0.8624999980881691286, -25.00000000000000000 ) ) ;
#3970 = DIRECTION ( 'NONE',  ( 0.000000000000000000, 1.000000000000000000, 0.000000000000000000 ) ) ;
#3971 = CARTESIAN_POINT ( 'NONE',  ( 10.35533905932737930, 0.1874999999999999722, -25.00000000000000000 ) ) ;
#3972 = FACE_OUTER_BOUND ( 'NONE', #2902, .T. ) ;
#3973 = EDGE_CURVE ( 'NONE', #8246, #3774, #1228, .T. ) ;
#3974 = VERTEX_POINT ( 'NONE', #8740 ) ;
#3975 = EDGE_LOOP ( 'NONE', ( #9001, #7339, #10556, #6118, #10077, #10933 ) ) ;
#3976 = ADVANCED_FACE ( 'NONE', ( #10448 ), #3016, .T. ) ;
#3977 = LINE ( 'NONE', #7328, #7413 ) ;
#3978 = FILL_AREA_STYLE ('',( #10036 ) ) ;
#3979 = CARTESIAN_POINT ( 'NONE',  ( -17.40975659021753330, 4.018749999044084475, 17.40975659021752975 ) ) ;
#3980 = ORIENTED_EDGE ( 'NONE', *, *, #10904, .F. ) ;
#3981 = CARTESIAN_POINT ( 'NONE',  ( 25.00000000000000000, 3.612499998088169129, 0.000000000000000000 ) ) ;
#3982 = PRODUCT_CONTEXT ( 'NONE', #330, 'mechanical' ) ;
#3983 = CARTESIAN_POINT ( 'NONE',  ( 6.123233995736763324E-16, 20.00000000000000355, 4.999999999999997335 ) ) ;
#3984 = ORIENTED_EDGE ( 'NONE', *, *, #10172, .T. ) ;
#3985 = DIRECTION ( 'NONE',  ( 0.000000000000000000, 1.000000000000000000, 0.000000000000000000 ) ) ;
#3986 = EDGE_LOOP ( 'NONE', ( #5307, #807, #8021, #891, #9823 ) ) ;
#3987 = ORIENTED_EDGE ( 'NONE', *, *, #2722, .T. ) ;
#3988 = ORIENTED_EDGE ( 'NONE', *, *, #5849, .F. ) ;
#3989 = EDGE_CURVE ( 'NONE', #4764, #3676, #7964, .T. ) ;
#3990 = CARTESIAN_POINT ( 'NONE',  ( 25.00000000000000000, 5.612499998088169129, 0.000000000000000000 ) ) ;
#3991 = DIRECTION ( 'NONE',  ( 0.000000000000000000, 0.000000000000000000, 1.000000000000000000 ) ) ;
#3992 = CARTESIAN_POINT ( 'NONE',  ( -24.62111388750000174, 1.656249999044084431, -10.19839929293506131 ) ) ;
#3993 = ORIENTED_EDGE ( 'NONE', *, *, #6744, .F. ) ;
#3994 = DIRECTION ( 'NONE',  ( 1.000000000000000000, 0.000000000000000000, -1.069128445102650095E-14 ) ) ;
#3995 = LINE ( 'NONE', #837, #3497 ) ;
#3996 = CARTESIAN_POINT ( 'NONE',  ( 17.67766952966368521, 1.487499998088169129, 17.67766952966369232 ) ) ;
#3997 = DIRECTION ( 'NONE',  ( 0.000000000000000000, 1.000000000000000000, 0.000000000000000000 ) ) ;
#3998 = PLANE ( 'NONE',  #2467 ) ;
#3999 = EDGE_LOOP ( 'NONE', ( #1105, #2772, #4507, #747, #6795 ) ) ;
#4000 = EDGE_LOOP ( 'NONE', ( #10494, #2128, #6033, #9987 ) ) ;
#4001 = VERTEX_POINT ( 'NONE', #7184 ) ;
#4002 = ORIENTED_EDGE ( 'NONE', *, *, #7682, .T. ) ;
#4003 = CARTESIAN_POINT ( 'NONE',  ( 1.507608415688466075E-15, 0.4687499990440845421, -24.62111388750000174 ) ) ;
#4004 = CARTESIAN_POINT ( 'NONE',  ( 3.644491357022480837, 19.66631150450990617, 5.978755702618567369 ) ) ;
#4005 = ORIENTED_EDGE ( 'NONE', *, *, #1213, .T. ) ;
#4006 = DIRECTION ( 'NONE',  ( 0.000000000000000000, -2.775557561562888270E-17, -1.000000000000000000 ) ) ;
#4007 = DIRECTION ( 'NONE',  ( 0.000000000000000000, 0.000000000000000000, -1.000000000000000000 ) ) ;
#4008 = CARTESIAN_POINT ( 'NONE',  ( -10.19839929293505776, 1.531249999044084653, -24.62111388750000174 ) ) ;
#4009 = CARTESIAN_POINT ( 'NONE',  ( 9.875000000000023093, 28.00000000000000000, 17.10400172474264835 ) ) ;
#4010 =( BOUNDED_CURVE ( )  B_SPLINE_CURVE ( 3, ( #863, #5124, #7714, #9246 ),
 .UNSPECIFIED., .F., .F. ) 
 B_SPLINE_CURVE_WITH_KNOTS ( ( 4, 4 ),
 ( 3.927175151554409549, 3.998664601439929189 ),
 .UNSPECIFIED. ) 
 CURVE ( )  GEOMETRIC_REPRESENTATION_ITEM ( )  RATIONAL_B_SPLINE_CURVE ( ( 1.000000000000000000, 0.9995741502243209453, 0.9995741502243209453, 1.000000000000000000 ) ) 
 REPRESENTATION_ITEM ( '' )  );
#4011 = EDGE_LOOP ( 'NONE', ( #8912, #5018, #8397, #3121 ) ) ;
#4012 = EDGE_LOOP ( 'NONE', ( #4268, #2607, #2311, #8044, #8095 ) ) ;
#4013 = EDGE_LOOP ( 'NONE', ( #1739, #8966, #1443, #537 ) ) ;
#4014 = ORIENTED_EDGE ( 'NONE', *, *, #2336, .T. ) ;
#4015 = CIRCLE ( 'NONE', #3673, 2.999999999999999112 ) ;
#4016 = CARTESIAN_POINT ( 'NONE',  ( -9.874999999999777955, 25.00000000000000000, 20.10400172474279401 ) ) ;
#4017 = EDGE_CURVE ( 'NONE', #10229, #6293, #9564, .T. ) ;
#4018 = CARTESIAN_POINT ( 'NONE',  ( 17.67766952966369232, 0.7374999980881691286, -17.67766952966369232 ) ) ;
#4019 = EDGE_CURVE ( 'NONE', #7282, #7845, #526, .T. ) ;
#4020 = PLANE ( 'NONE',  #6753 ) ;
#4021 = CARTESIAN_POINT ( 'NONE',  ( 1.530808498934191521E-15, 1.250000000000000000, -25.00000000000000000 ) ) ;
#4022 = FACE_BOUND ( 'NONE', #4780, .T. ) ;
#4023 = ADVANCED_FACE ( 'NONE', ( #5426 ), #8838, .T. ) ;
#4024 = EDGE_CURVE ( 'NONE', #3774, #6423, #2148, .T. ) ;
#4025 = EDGE_LOOP ( 'NONE', ( #7691, #6152, #7634, #10615 ) ) ;
#4026 = DIRECTION ( 'NONE',  ( 0.000000000000000000, 1.000000000000000000, -0.000000000000000000 ) ) ;
#4027 = VECTOR ( 'NONE', #6542, 1000.000000000000000 ) ;
#4028 = CARTESIAN_POINT ( 'NONE',  ( 17.40975659021752975, 3.518749999044084920, -17.40975659021752975 ) ) ;
#4029 = VERTEX_POINT ( 'NONE', #8786 ) ;
#4030 = EDGE_CURVE ( 'NONE', #4797, #9038, #4068, .T. ) ;
#4031 = FACE_OUTER_BOUND ( 'NONE', #219, .T. ) ;
#4032 = CARTESIAN_POINT ( 'NONE',  ( 0.000000000000000000, 0.000000000000000000, 0.000000000000000000 ) ) ;
#4033 = CARTESIAN_POINT ( 'NONE',  ( 8.660254037844401509, 95.00000000000001421, -5.000000000000000000 ) ) ;
#4034 = VERTEX_POINT ( 'NONE', #2007 ) ;
#4035 = AXIS2_PLACEMENT_3D ( 'NONE', #5166, #4332, #8515 ) ;
#4036 = CARTESIAN_POINT ( 'NONE',  ( 67.97877056362573001, 94.28203230275514102, -5.000000000000000000 ) ) ;
#4037 = CARTESIAN_POINT ( 'NONE',  ( -24.62111388750000174, 1.718749999044084431, -3.015216831376932151E-15 ) ) ;
#4038 = ORIENTED_EDGE ( 'NONE', *, *, #9277, .T. ) ;
#4039 = ADVANCED_FACE ( 'NONE', ( #3708 ), #4609, .F. ) ;
#4040 = ORIENTED_EDGE ( 'NONE', *, *, #688, .F. ) ;
#4041 = VERTEX_POINT ( 'NONE', #6418 ) ;
#4042 = CARTESIAN_POINT ( 'NONE',  ( 17.40975659021752620, 1.268749999044084475, 17.40975659021753330 ) ) ;
#4043 = DIRECTION ( 'NONE',  ( 0.000000000000000000, 0.000000000000000000, -1.000000000000000000 ) ) ;
#4044 = CARTESIAN_POINT ( 'NONE',  ( -24.62111388750000884, 0.7812499990440845421, 10.19839929293505421 ) ) ;
#4045 = ORIENTED_EDGE ( 'NONE', *, *, #9634, .F. ) ;
#4046 = DIRECTION ( 'NONE',  ( 1.000000000000000000, 0.000000000000000000, 0.000000000000000000 ) ) ;
#4047 = CARTESIAN_POINT ( 'NONE',  ( -6.296693311223937606, 19.03096903053434019, 3.058047309049956031 ) ) ;
#4048 = DIRECTION ( 'NONE',  ( -0.000000000000000000, 1.000000000000000000, 0.000000000000000000 ) ) ;
#4049 = CARTESIAN_POINT ( 'NONE',  ( -3.957930336368489021E-15, 25.00000000000000000, -19.75000000000000000 ) ) ;
#4050 = LINE ( 'NONE', #1553, #5469 ) ;
#4051 = EDGE_CURVE ( 'NONE', #5286, #9729, #7141, .T. ) ;
#4052 = ORIENTED_EDGE ( 'NONE', *, *, #9364, .F. ) ;
#4053 = ORIENTED_EDGE ( 'NONE', *, *, #5144, .T. ) ;
#4054 = ORIENTED_EDGE ( 'NONE', *, *, #7488, .T. ) ;
#4055 = PRODUCT_DEFINITION_CONTEXT ( 'detailed design', #10061, 'design' ) ;
#4056 = CARTESIAN_POINT ( 'NONE',  ( 17.40975659021752620, 1.093749999044084653, 17.40975659021753330 ) ) ;
#4057 = FACE_OUTER_BOUND ( 'NONE', #3415, .T. ) ;
#4058 = AXIS2_PLACEMENT_3D ( 'NONE', #2823, #5486, #8850 ) ;
#4059 = AXIS2_PLACEMENT_3D ( 'NONE', #9530, #1086, #9586 ) ;
#4060 = ORIENTED_EDGE ( 'NONE', *, *, #4211, .F. ) ;
#4061 = DIRECTION ( 'NONE',  ( 0.000000000000000000, -1.000000000000000000, 0.000000000000000000 ) ) ;
#4062 = DIRECTION ( 'NONE',  ( 0.000000000000000000, 0.000000000000000000, -1.000000000000000000 ) ) ;
#4063 = CARTESIAN_POINT ( 'NONE',  ( 17.40975659021752620, 1.093749999044084653, 17.40975659021753330 ) ) ;
#4064 = DIRECTION ( 'NONE',  ( 0.000000000000000000, -1.000000000000000000, 0.000000000000000000 ) ) ;
#4065 = EDGE_LOOP ( 'NONE', ( #2508, #4424, #10294, #4228, #7222 ) ) ;
#4066 = EDGE_LOOP ( 'NONE', ( #6705, #9615, #7809, #4896 ) ) ;
#4067 = ORIENTED_EDGE ( 'NONE', *, *, #6130, .F. ) ;
#4068 = CIRCLE ( 'NONE', #9348, 5.525000000000006573 ) ;
#4069 = CIRCLE ( 'NONE', #703, 2.999999999999999112 ) ;
#4070 = VERTEX_POINT ( 'NONE', #6306 ) ;
#4071 = CARTESIAN_POINT ( 'NONE',  ( 27.60306914047445304, 97.85373563005803987, -5.000000000000000000 ) ) ;
#4072 = LINE ( 'NONE', #7218, #9936 ) ;
#4073 = CARTESIAN_POINT ( 'NONE',  ( 1.530808498934191521E-15, 4.862499998088169129, -25.00000000000000000 ) ) ;
#4074 = VECTOR ( 'NONE', #3777, 1000.000000000000000 ) ;
#4075 = COLOUR_RGB ( '', 0.31764706, 0.68627451, 0.89019608) ;
#4076 =( BOUNDED_CURVE ( )  B_SPLINE_CURVE ( 3, ( #403, #8023, #7149, #3824 ),
 .UNSPECIFIED., .F., .F. ) 
 B_SPLINE_CURVE_WITH_KNOTS ( ( 4, 4 ),
 ( 2.284520705739656155, 2.356010155625177127 ),
 .UNSPECIFIED. ) 
 CURVE ( )  GEOMETRIC_REPRESENTATION_ITEM ( )  RATIONAL_B_SPLINE_CURVE ( ( 1.000000000000000000, 0.9995741502243209453, 0.9995741502243209453, 1.000000000000000000 ) ) 
 REPRESENTATION_ITEM ( '' )  );
#4077 = CARTESIAN_POINT ( 'NONE',  ( -15.75000000000003553, 28.00000000000000000, -2.999999999999832578 ) ) ;
#4078 = CARTESIAN_POINT ( 'NONE',  ( 2.500000000000000444, -1.000000000000003109, -0.5773502691896260641 ) ) ;
#4079 = VERTEX_POINT ( 'NONE', #1327 ) ;
#4080 = DIRECTION ( 'NONE',  ( 0.2500000000000041078, 0.8660254037844380415, -0.4330127018922182436 ) ) ;
#4081 = SURFACE_STYLE_USAGE ( .BOTH. , #5787 ) ;
#4082 = AXIS2_PLACEMENT_3D ( 'NONE', #9184, #9905, #4952 ) ;
#4083 = CARTESIAN_POINT ( 'NONE',  ( -24.62111388750000174, 0.8312499990440843645, -10.19839929293506131 ) ) ;
#4084 = ORIENTED_EDGE ( 'NONE', *, *, #8149, .T. ) ;
#4085 = DIRECTION ( 'NONE',  ( 0.000000000000000000, -0.000000000000000000, 1.000000000000000000 ) ) ;
#4086 = LINE ( 'NONE', #10764, #54 ) ;
#4087 = VERTEX_POINT ( 'NONE', #4708 ) ;
#4088 = FACE_OUTER_BOUND ( 'NONE', #10572, .T. ) ;
#4089 = CARTESIAN_POINT ( 'NONE',  ( 24.62111388750000174, 2.218749999044084653, 0.000000000000000000 ) ) ;
#4090 = ORIENTED_EDGE ( 'NONE', *, *, #3757, .F. ) ;
#4091 = ORIENTED_EDGE ( 'NONE', *, *, #2357, .F. ) ;
#4092 = VECTOR ( 'NONE', #3785, 1000.000000000000114 ) ;
#4093 = EDGE_CURVE ( 'NONE', #631, #4112, #8056, .T. ) ;
#4094 = ADVANCED_FACE ( 'NONE', ( #4508 ), #287, .T. ) ;
#4095 = ORIENTED_EDGE ( 'NONE', *, *, #1153, .T. ) ;
#4096 = EDGE_CURVE ( 'NONE', #2617, #387, #2363, .T. ) ;
#4097 = CARTESIAN_POINT ( 'NONE',  ( -4.592425496802574367E-15, 4.362499998088169129, 25.00000000000000000 ) ) ;
#4098 = CARTESIAN_POINT ( 'NONE',  ( 12.47307621135322186, 28.00000000000000000, -15.60400172474273717 ) ) ;
#4099 = CARTESIAN_POINT ( 'NONE',  ( -17.40975659021752975, 2.593749999044084653, -17.40975659021752975 ) ) ;
#4100 = VERTEX_POINT ( 'NONE', #7502 ) ;
#4101 = DIRECTION ( 'NONE',  ( 1.069128445102650095E-14, 0.000000000000000000, 1.000000000000000000 ) ) ;
#4102 = EDGE_CURVE ( 'NONE', #7345, #1671, #3171, .T. ) ;
#4103 = CARTESIAN_POINT ( 'NONE',  ( -10.35533905932739174, 4.299999998088169129, 24.99999999999999289 ) ) ;
#4104 = CARTESIAN_POINT ( 'NONE',  ( -17.67766952966369232, 2.237499998088169573, 17.67766952966368876 ) ) ;
#4105 = CARTESIAN_POINT ( 'NONE',  ( 0.000000000000000000, 10.00000000000000355, 0.000000000000000000 ) ) ;
#4106 = CARTESIAN_POINT ( 'NONE',  ( -3.924072712834500543, 19.03096903053431177, 5.796693311223878098 ) ) ;
#4107 = DIRECTION ( 'NONE',  ( 0.000000000000000000, 0.000000000000000000, 1.000000000000000000 ) ) ;
#4108 = AXIS2_PLACEMENT_3D ( 'NONE', #9428, #2778, #6959 ) ;
#4109 = AXIS2_PLACEMENT_3D ( 'NONE', #7729, #881, #7792 ) ;
#4110 = ORIENTED_EDGE ( 'NONE', *, *, #7453, .T. ) ;
#4111 = EDGE_CURVE ( 'NONE', #9754, #2886, #2564, .T. ) ;
#4112 = VERTEX_POINT ( 'NONE', #3117 ) ;
#4113 = CIRCLE ( 'NONE', #5518, 25.00000000000000000 ) ;
#4114 = AXIS2_PLACEMENT_3D ( 'NONE', #5095, #5922, #9271 ) ;
#4115 = DIRECTION ( 'NONE',  ( -0.000000000000000000, -1.000000000000000000, -0.000000000000000000 ) ) ;
#4116 = FILL_AREA_STYLE ('',( #9180 ) ) ;
#4117 = AXIS2_PLACEMENT_3D ( 'NONE', #9448, #8494, #5964 ) ;
#4118 = EDGE_CURVE ( 'NONE', #387, #1232, #5131, .T. ) ;
#4119 = CARTESIAN_POINT ( 'NONE',  ( 7.276923788646707969, 28.00000000000000000, 18.60400172474265190 ) ) ;
#4120 = DIRECTION ( 'NONE',  ( 0.000000000000000000, -0.000000000000000000, 1.000000000000000000 ) ) ;
#4121 = CARTESIAN_POINT ( 'NONE',  ( 0.000000000000000000, 10.00000000000000355, 0.000000000000000000 ) ) ;
#4122 = CARTESIAN_POINT ( 'NONE',  ( -24.62111388750000174, 0.6562499990440846531, -10.19839929293506131 ) ) ;
#4123 = CARTESIAN_POINT ( 'NONE',  ( 2.632990618166809235E-16, 20.00000000000000355, 2.149999999999999911 ) ) ;
#4124 = ORIENTED_EDGE ( 'NONE', *, *, #6344, .F. ) ;
#4125 = AXIS2_PLACEMENT_3D ( 'NONE', #6667, #10026, #2448 ) ;
#4126 = ORIENTED_EDGE ( 'NONE', *, *, #1814, .T. ) ;
#4127 = ORIENTED_EDGE ( 'NONE', *, *, #4903, .T. ) ;
#4128 = ORIENTED_EDGE ( 'NONE', *, *, #8947, .T. ) ;
#4129 = AXIS2_PLACEMENT_3D ( 'NONE', #8373, #4295, #1747 ) ;
#4130 = DIRECTION ( 'NONE',  ( -1.000000000000000000, 0.000000000000000000, 0.000000000000000000 ) ) ;
#4131 = AXIS2_PLACEMENT_3D ( 'NONE', #3793, #7165, #2729 ) ;
#4132 = FACE_BOUND ( 'NONE', #443, .T. ) ;
#4133 = DIRECTION ( 'NONE',  ( 0.000000000000000000, 0.000000000000000000, 1.000000000000000000 ) ) ;
#4134 = DIRECTION ( 'NONE',  ( 0.8660254037844399289, 0.000000000000000000, 0.4999999999999978351 ) ) ;
#4135 = CARTESIAN_POINT ( 'NONE',  ( 0.000000000000000000, 28.00000000000000000, -10.50000000000000000 ) ) ;
#4136 = ORIENTED_EDGE ( 'NONE', *, *, #9583, .T. ) ;
#4137 = ORIENTED_EDGE ( 'NONE', *, *, #453, .T. ) ;
#4138 = EDGE_CURVE ( 'NONE', #528, #2606, #604, .T. ) ;
#4139 = LINE ( 'NONE', #4358, #5627 ) ;
#4140 = FILL_AREA_STYLE ('',( #1698 ) ) ;
#4141 = CARTESIAN_POINT ( 'NONE',  ( 0.2251666049839524120, 0.000000000000000000, -2.000000000000004441 ) ) ;
#4142 = DIRECTION ( 'NONE',  ( 0.000000000000000000, 2.775557561562888270E-17, 1.000000000000000000 ) ) ;
#4143 = ORIENTED_EDGE ( 'NONE', *, *, #4218, .T. ) ;
#4144 = DIRECTION ( 'NONE',  ( 0.000000000000000000, 0.000000000000000000, -1.000000000000000000 ) ) ;
#4145 = CARTESIAN_POINT ( 'NONE',  ( 82.32050807568876394, 99.93473594742127375, 0.000000000000000000 ) ) ;
#4146 = DIRECTION ( 'NONE',  ( 0.2499999999999979738, -0.8660254037844380415, 0.4330127018922216853 ) ) ;
#4147 = CARTESIAN_POINT ( 'NONE',  ( 10.19839929293506486, 1.031249999044084653, 24.62111388749999819 ) ) ;
#4148 = VERTEX_POINT ( 'NONE', #6512 ) ;
#4149 = CARTESIAN_POINT ( 'NONE',  ( 10.19839929293506486, 1.206249999044084698, 24.62111388749999819 ) ) ;
#4150 = CARTESIAN_POINT ( 'NONE',  ( 0.000000000000000000, 25.00000000000000000, -25.00000000000000000 ) ) ;
#4151 = CARTESIAN_POINT ( 'NONE',  ( -10.19839929293507552, 1.906249999044084431, 24.62111388749999463 ) ) ;
#4152 = CARTESIAN_POINT ( 'NONE',  ( 1.499999999999999556, 88.00000000000001421, -1.500000000000000222 ) ) ;
#4153 = ORIENTED_EDGE ( 'NONE', *, *, #8898, .T. ) ;
#4154 = CARTESIAN_POINT ( 'NONE',  ( 3.957930336368489021E-15, 28.00000000000000000, 19.75000000000000000 ) ) ;
#4155 = DIRECTION ( 'NONE',  ( 0.000000000000000000, 1.000000000000000000, 0.000000000000000000 ) ) ;
#4156 = EDGE_CURVE ( 'NONE', #10414, #2208, #1249, .T. ) ;
#4157 = DIRECTION ( 'NONE',  ( 1.000000000000000000, 0.000000000000000000, -3.708321773340234242E-15 ) ) ;
#4158 = CARTESIAN_POINT ( 'NONE',  ( 1.500000000000000000, 88.00000000000001421, 1.500000000000000000 ) ) ;
#4159 = DIRECTION ( 'NONE',  ( -1.000000000000000000, -0.000000000000000000, -7.228014483236695816E-17 ) ) ;
#4160 = DIRECTION ( 'NONE',  ( -0.4999999999999887312, 0.000000000000000000, 0.8660254037844451469 ) ) ;
#4161 = ORIENTED_EDGE ( 'NONE', *, *, #1929, .T. ) ;
#4162 = ORIENTED_EDGE ( 'NONE', *, *, #106, .T. ) ;
#4163 = EDGE_CURVE ( 'NONE', #689, #10532, #768, .T. ) ;
#4164 = CARTESIAN_POINT ( 'NONE',  ( 24.99999999999999289, 5.549999998088169129, 10.35533905932739529 ) ) ;
#4165 = CARTESIAN_POINT ( 'NONE',  ( 10.19839929293505953, 1.406249999044084653, -24.62111388750000174 ) ) ;
#4166 = CARTESIAN_POINT ( 'NONE',  ( 6.982120021884469452, 10.00000000000000355, -0.4999999999999756306 ) ) ;
#4167 = EDGE_CURVE ( 'NONE', #806, #9105, #5790, .T. ) ;
#4168 = CARTESIAN_POINT ( 'NONE',  ( 4.895565917430008795, 5.000000000000001776, 24.12949820052922334 ) ) ;
#4169 = DIRECTION ( 'NONE',  ( -0.7071067811865457964, 0.000000000000000000, 0.7071067811865492381 ) ) ;
#4170 = CARTESIAN_POINT ( 'NONE',  ( -24.62111388750000884, 2.781249999044085541, 10.19839929293505421 ) ) ;
#4171 = DIRECTION ( 'NONE',  ( 0.000000000000000000, 0.000000000000000000, 1.000000000000000000 ) ) ;
#4172 = ORIENTED_EDGE ( 'NONE', *, *, #5717, .T. ) ;
#4173 = ORIENTED_EDGE ( 'NONE', *, *, #7132, .T. ) ;
#4174 = ORIENTED_EDGE ( 'NONE', *, *, #7002, .T. ) ;
#4175 = ADVANCED_FACE ( 'NONE', ( #9816 ), #9151, .T. ) ;
#4176 = ORIENTED_EDGE ( 'NONE', *, *, #3505, .F. ) ;
#4177 = CARTESIAN_POINT ( 'NONE',  ( -0.5000000000000000000, 10.00000000000000355, 5.999999999999998224 ) ) ;
#4178 = CARTESIAN_POINT ( 'NONE',  ( -10.47307621135341904, 28.00000000000000000, -12.13990010960482557 ) ) ;
#4179 = FACE_OUTER_BOUND ( 'NONE', #660, .T. ) ;
#4180 = CARTESIAN_POINT ( 'NONE',  ( 0.000000000000000000, 5.000000000000000000, 0.000000000000000000 ) ) ;
#4181 = CARTESIAN_POINT ( 'NONE',  ( 24.72166399154381011, 4.999999999999999112, 3.527620825298249052 ) ) ;
#4182 = EDGE_CURVE ( 'NONE', #9832, #1988, #706, .T. ) ;
#4183 = ORIENTED_EDGE ( 'NONE', *, *, #1455, .T. ) ;
#4184 = CARTESIAN_POINT ( 'NONE',  ( 0.000000000000000000, 10.00000000000000355, 0.000000000000000000 ) ) ;
#4185 = DIRECTION ( 'NONE',  ( 0.000000000000000000, -1.000000000000000000, 0.000000000000000000 ) ) ;
#4186 = CARTESIAN_POINT ( 'NONE',  ( 3.924072712834419718, 19.03096903053430466, 5.796693311223933165 ) ) ;
#4187 = DIRECTION ( 'NONE',  ( 0.2499999999999949762, 0.8660254037844380415, 0.4330127018922234061 ) ) ;
#4188 = EDGE_LOOP ( 'NONE', ( #9158, #4638, #9295, #418 ) ) ;
#4189 = DIRECTION ( 'NONE',  ( 2.168404344971010347E-16, 0.000000000000000000, 1.000000000000000000 ) ) ;
#4190 = SHAPE_DEFINITION_REPRESENTATION ( #1953, #2382 ) ;
#4191 = CARTESIAN_POINT ( 'NONE',  ( 0.000000000000000000, 85.00000000000000000, -25.00000000000000000 ) ) ;
#4192 = AXIS2_PLACEMENT_3D ( 'NONE', #10931, #2512, #5904 ) ;
#4193 = FACE_OUTER_BOUND ( 'NONE', #3423, .T. ) ;
#4194 = CARTESIAN_POINT ( 'NONE',  ( -4.522825247065398226E-15, 3.968749999044084209, 24.62111388750000174 ) ) ;
#4195 = VECTOR ( 'NONE', #8534, 1000.000000000000000 ) ;
#4196 = ORIENTED_EDGE ( 'NONE', *, *, #7843, .F. ) ;
#4197 =( GEOMETRIC_REPRESENTATION_CONTEXT ( 3 ) GLOBAL_UNCERTAINTY_ASSIGNED_CONTEXT ( ( #4843 ) ) GLOBAL_UNIT_ASSIGNED_CONTEXT ( ( #1730, #8459, #10907 ) ) REPRESENTATION_CONTEXT ( 'NONE', 'WORKASPACE' ) );
#4198 = CARTESIAN_POINT ( 'NONE',  ( -4.522825247065398226E-15, 2.143749999044084920, 24.62111388750000174 ) ) ;
#4199 = CARTESIAN_POINT ( 'NONE',  ( 19.75000000000001066, 25.00000000000000000, 2.999999999999927613 ) ) ;
#4200 = CARTESIAN_POINT ( 'NONE',  ( -24.62111388750000174, 2.656249999044085097, -10.19839929293506131 ) ) ;
#4201 = CARTESIAN_POINT ( 'NONE',  ( 0.000000000000000000, 0.000000000000000000, -1.610000000000003872 ) ) ;
#4202 = ORIENTED_EDGE ( 'NONE', *, *, #3076, .F. ) ;
#4203 = CARTESIAN_POINT ( 'NONE',  ( -10.35533905932739174, 3.687500000000000444, 24.99999999999999289 ) ) ;
#4204 = FACE_OUTER_BOUND ( 'NONE', #4707, .T. ) ;
#4205 = DIRECTION ( 'NONE',  ( -0.000000000000000000, -1.000000000000000000, -0.000000000000000000 ) ) ;
#4206 = CARTESIAN_POINT ( 'NONE',  ( 3.061616997868383043E-15, 85.00000000000000000, 25.00000000000000000 ) ) ;
#4207 = CARTESIAN_POINT ( 'NONE',  ( 0.000000000000000000, 0.000000000000000000, -28.00000000000000000 ) ) ;
#4208 = EDGE_LOOP ( 'NONE', ( #3302, #8020, #383, #5555, #3221, #677, #4161, #5362, #549, #9118, #8591, #10076, #2549, #1371, #10938, #4939, #5565 ) ) ;
#4209 = EDGE_LOOP ( 'NONE', ( #4110, #870, #597, #6691 ) ) ;
#4210 = ORIENTED_EDGE ( 'NONE', *, *, #8400, .F. ) ;
#4211 = EDGE_CURVE ( 'NONE', #5713, #2855, #7948, .T. ) ;
#4212 = DIRECTION ( 'NONE',  ( 0.000000000000000000, 0.000000000000000000, 1.000000000000000000 ) ) ;
#4213 = CARTESIAN_POINT ( 'NONE',  ( 24.62111388750000174, 4.393749999044085364, 0.000000000000000000 ) ) ;
#4214 = CARTESIAN_POINT ( 'NONE',  ( -10.19839929293507552, 2.081249999044084475, 24.62111388749999463 ) ) ;
#4215 = CARTESIAN_POINT ( 'NONE',  ( 24.62111388749999463, 2.156249999044085097, 10.19839929293507730 ) ) ;
#4216 = CYLINDRICAL_SURFACE ( 'NONE', #9308, 2.000000000000004441 ) ;
#4217 = CARTESIAN_POINT ( 'NONE',  ( -4.592425496802574367E-15, 2.362499998088169129, 25.00000000000000000 ) ) ;
#4218 = EDGE_CURVE ( 'NONE', #7303, #10062, #3329, .T. ) ;
#4219 = CARTESIAN_POINT ( 'NONE',  ( 10.35533905932738286, 4.424999998088169129, 24.99999999999999645 ) ) ;
#4220 = CARTESIAN_POINT ( 'NONE',  ( 17.67766952966369232, 1.125000000000000222, -17.67766952966369232 ) ) ;
#4221 = CARTESIAN_POINT ( 'NONE',  ( 25.10306914047445659, 102.1838626489802380, -5.000000000000000000 ) ) ;
#4222 = ORIENTED_EDGE ( 'NONE', *, *, #3624, .F. ) ;
#4223 = ORIENTED_EDGE ( 'NONE', *, *, #6731, .F. ) ;
#4224 = ORIENTED_EDGE ( 'NONE', *, *, #1199, .T. ) ;
#4225 = ORIENTED_EDGE ( 'NONE', *, *, #7734, .T. ) ;
#4226 = ADVANCED_FACE ( 'NONE', ( #5581 ), #1485, .F. ) ;
#4227 = EDGE_CURVE ( 'NONE', #8104, #10668, #8938, .T. ) ;
#4228 = ORIENTED_EDGE ( 'NONE', *, *, #9500, .F. ) ;
#4229 = VECTOR ( 'NONE', #8226, 1000.000000000000000 ) ;
#4230 = AXIS2_PLACEMENT_3D ( 'NONE', #6326, #2112, #5493 ) ;
#4231 = CARTESIAN_POINT ( 'NONE',  ( -10.47307621135315792, -0.001000000000001000089, 12.13990010960504762 ) ) ;
#4232 = SHAPE_REPRESENTATION ( 'Lower Catch Container', ( #7040 ), #8059 ) ;
#4233 = DIRECTION ( 'NONE',  ( -0.8660254037844328234, 0.000000000000000000, 0.5000000000000098810 ) ) ;
#4234 = EDGE_CURVE ( 'NONE', #5714, #3931, #6465, .T. ) ;
#4235 = CARTESIAN_POINT ( 'NONE',  ( 17.67766952966368521, 4.875000000000000000, 17.67766952966369232 ) ) ;
#4236 = CARTESIAN_POINT ( 'NONE',  ( 12.13990010960493748, 28.00000000000000000, 10.47307621135328759 ) ) ;
#4237 = DIRECTION ( 'NONE',  ( 0.000000000000000000, 0.000000000000000000, 1.000000000000000000 ) ) ;
#4238 = VECTOR ( 'NONE', #7283, 1000.000000000000114 ) ;
#4239 = AXIS2_PLACEMENT_3D ( 'NONE', #4876, #7397, #5040 ) ;
#4240 = ADVANCED_FACE ( 'NONE', ( #4031 ), #2248, .F. ) ;
#4241 = EDGE_LOOP ( 'NONE', ( #8135, #6779, #3361, #3184, #3934 ) ) ;
#4242 = VECTOR ( 'NONE', #3611, 1000.000000000000000 ) ;
#4243 = DIRECTION ( 'NONE',  ( 0.4999999999999949485, 0.000000000000000000, 0.8660254037844415942 ) ) ;
#4244 = DIRECTION ( 'NONE',  ( 1.000000000000000000, 0.000000000000000000, 0.000000000000000000 ) ) ;
#4245 = CIRCLE ( 'NONE', #5663, 2.999999999999997335 ) ;
#4246 = CARTESIAN_POINT ( 'NONE',  ( 0.000000000000000000, 0.000000000000000000, -1.610000000000000320 ) ) ;
#4247 = ORIENTED_EDGE ( 'NONE', *, *, #4024, .T. ) ;
#4248 = CARTESIAN_POINT ( 'NONE',  ( 0.000000000000000000, 10.00000000000000355, 0.000000000000000000 ) ) ;
#4249 = ADVANCED_FACE ( 'NONE', ( #8490 ), #825, .T. ) ;
#4250 = CARTESIAN_POINT ( 'NONE',  ( 3.429011037612589276E-15, 85.00000000000000000, 28.00000000000000000 ) ) ;
#4251 = CYLINDRICAL_SURFACE ( 'NONE', #7203, 7.500000000000000888 ) ;
#4252 = CIRCLE ( 'NONE', #10431, 7.500000000000007994 ) ;
#4253 = ORIENTED_EDGE ( 'NONE', *, *, #9275, .T. ) ;
#4254 = CIRCLE ( 'NONE', #3167, 7.400000000000007461 ) ;
#4255 = CARTESIAN_POINT ( 'NONE',  ( -24.62111388750000174, 0.8312499990440845865, -10.19839929293506131 ) ) ;
#4256 = CARTESIAN_POINT ( 'NONE',  ( 17.40975659021752620, 2.268749999044084475, 17.40975659021753330 ) ) ;
#4257 = DIRECTION ( 'NONE',  ( 1.000000000000000000, 0.000000000000000000, 0.000000000000000000 ) ) ;
#4258 = LINE ( 'NONE', #55, #1534 ) ;
#4259 = CARTESIAN_POINT ( 'NONE',  ( 28.89716436598705585, 102.6833647615033840, 5.000000000000000000 ) ) ;
#4260 = CYLINDRICAL_SURFACE ( 'NONE', #2282, 25.00000000000000000 ) ;
#4261 = FACE_OUTER_BOUND ( 'NONE', #471, .T. ) ;
#4262 = PLANE ( 'NONE',  #6505 ) ;
#4263 = DIRECTION ( 'NONE',  ( -0.000000000000000000, -1.000000000000000000, -0.000000000000000000 ) ) ;
#4264 = CARTESIAN_POINT ( 'NONE',  ( 1.500000000000001332, 0.000000000000000000, 0.000000000000000000 ) ) ;
#4265 = VECTOR ( 'NONE', #8526, 1000.000000000000000 ) ;
#4266 = VERTEX_POINT ( 'NONE', #220 ) ;
#4267 = ORIENTED_EDGE ( 'NONE', *, *, #4582, .T. ) ;
#4268 = ORIENTED_EDGE ( 'NONE', *, *, #3060, .F. ) ;
#4269 = ORIENTED_EDGE ( 'NONE', *, *, #3634, .T. ) ;
#4270 = DIRECTION ( 'NONE',  ( 0.000000000000000000, 0.000000000000000000, -1.000000000000000000 ) ) ;
#4271 = CARTESIAN_POINT ( 'NONE',  ( -17.40975659021753330, 4.018749999044084475, 17.40975659021752975 ) ) ;
#4272 = VECTOR ( 'NONE', #3299, 1000.000000000000000 ) ;
#4273 = DIRECTION ( 'NONE',  ( 1.000000000000000000, -0.000000000000000000, -0.000000000000000000 ) ) ;
#4274 = CARTESIAN_POINT ( 'NONE',  ( 24.62111388750000174, 1.456249999044084475, -10.19839929293505776 ) ) ;
#4275 = CARTESIAN_POINT ( 'NONE',  ( 25.00000000000000000, 1.000000000000000000, 0.000000000000000000 ) ) ;
#4276 = LINE ( 'NONE', #3370, #5088 ) ;
#4277 = ORIENTED_EDGE ( 'NONE', *, *, #7935, .T. ) ;
#4278 = DIRECTION ( 'NONE',  ( 0.000000000000000000, 1.000000000000000000, 0.000000000000000000 ) ) ;
#4279 = VECTOR ( 'NONE', #2005, 1000.000000000000000 ) ;
#4280 = CARTESIAN_POINT ( 'NONE',  ( -17.67766952966368876, 1.987499998088169129, -17.67766952966369232 ) ) ;
#4281 = CARTESIAN_POINT ( 'NONE',  ( 17.67766952966369232, 4.737499998088169129, -17.67766952966369232 ) ) ;
#4282 = CARTESIAN_POINT ( 'NONE',  ( 17.67766952966368521, 0.8750000000000000000, 17.67766952966369232 ) ) ;
#4283 = CARTESIAN_POINT ( 'NONE',  ( -10.35533905932737575, 2.924999998088169129, -25.00000000000000000 ) ) ;
#4284 = AXIS2_PLACEMENT_3D ( 'NONE', #6177, #7715, #3736 ) ;
#4285 = ORIENTED_EDGE ( 'NONE', *, *, #8359, .F. ) ;
#4286 = CIRCLE ( 'NONE', #2854, 2.999999999999996447 ) ;
#4287 = ORIENTED_EDGE ( 'NONE', *, *, #8335, .F. ) ;
#4288 = EDGE_LOOP ( 'NONE', ( #6425, #141, #7123, #8211 ) ) ;
#4289 = CIRCLE ( 'NONE', #940, 2.999999999999998668 ) ;
#4290 = FACE_OUTER_BOUND ( 'NONE', #4241, .T. ) ;
#4291 = AXIS2_PLACEMENT_3D ( 'NONE', #7056, #10412, #5401 ) ;
#4292 = CARTESIAN_POINT ( 'NONE',  ( 1.745740669421566678E-15, 0.000000000000000000, -0.5000000000000000000 ) ) ;
#4293 = ORIENTED_EDGE ( 'NONE', *, *, #9215, .T. ) ;
#4294 = CARTESIAN_POINT ( 'NONE',  ( 10.35533905932737930, 2.187500000000000444, -25.00000000000000000 ) ) ;
#4295 = DIRECTION ( 'NONE',  ( 0.000000000000000000, 1.000000000000000000, 0.000000000000000000 ) ) ;
#4296 = DIRECTION ( 'NONE',  ( -0.8660254037844344888, 0.000000000000000000, 0.5000000000000074385 ) ) ;
#4297 = EDGE_CURVE ( 'NONE', #9541, #3898, #5655, .T. ) ;
#4298 = CARTESIAN_POINT ( 'NONE',  ( 3.000000000000000888, -0.001000000000001000089, 15.75000000000000355 ) ) ;
#4299 = CARTESIAN_POINT ( 'NONE',  ( 9.874999999999895195, 25.00000000000000000, -17.10400172474272651 ) ) ;
#4300 = COLOUR_RGB ( '', 0.40784314, 0.44705882, 0.49803922) ;
#4301 = AXIS2_PLACEMENT_3D ( 'NONE', #5625, #10698, #7320 ) ;
#4302 = EDGE_CURVE ( 'NONE', #5017, #5745, #1053, .T. ) ;
#4303 = ORIENTED_EDGE ( 'NONE', *, *, #7096, .T. ) ;
#4304 = VECTOR ( 'NONE', #8982, 1000.000000000000000 ) ;
#4305 = DIRECTION ( 'NONE',  ( 0.000000000000000000, 0.000000000000000000, 1.000000000000000000 ) ) ;
#4306 = CARTESIAN_POINT ( 'NONE',  ( 6.999999999999999112, 10.00000000000000355, -0.4999999999999756306 ) ) ;
#4307 = CARTESIAN_POINT ( 'NONE',  ( 24.62111388750000174, 0.3937499990440845310, 0.000000000000000000 ) ) ;
#4308 = CARTESIAN_POINT ( 'NONE',  ( -12.47307621135311351, 25.00000000000000000, 15.60400172474282599 ) ) ;
#4309 = CONTEXT_DEPENDENT_SHAPE_REPRESENTATION ( #5212, #10505 ) ;
#4310 = DIRECTION ( 'NONE',  ( -0.000000000000000000, -1.000000000000000000, -0.000000000000000000 ) ) ;
#4311 = VECTOR ( 'NONE', #3641, 1000.000000000000000 ) ;
#4312 = PLANE ( 'NONE',  #4109 ) ;
#4313 = EDGE_CURVE ( 'NONE', #2818, #2407, #1578, .T. ) ;
#4314 = FACE_OUTER_BOUND ( 'NONE', #10031, .T. ) ;
#4315 = EDGE_CURVE ( 'NONE', #3378, #8379, #3403, .T. ) ;
#4316 = CARTESIAN_POINT ( 'NONE',  ( 1.507608415688466075E-15, 0.6437499990440845865, -24.62111388750000174 ) ) ;
#4317 = CARTESIAN_POINT ( 'NONE',  ( 10.19839929293506486, 2.206249999044084920, 24.62111388749999819 ) ) ;
#4318 = PLANE ( 'NONE',  #4777 ) ;
#4319 = CYLINDRICAL_SURFACE ( 'NONE', #4373, 5.750000000000006217 ) ;
#4320 = DIRECTION ( 'NONE',  ( 0.000000000000000000, 0.000000000000000000, -1.000000000000000000 ) ) ;
#4321 = VERTEX_POINT ( 'NONE', #9380 ) ;
#4322 = CARTESIAN_POINT ( 'NONE',  ( 9.874999999999895195, -0.001000000000001000089, -17.10400172474272651 ) ) ;
#4323 = CYLINDRICAL_SURFACE ( 'NONE', #8333, 25.00000000000000000 ) ;
#4324 = DIRECTION ( 'NONE',  ( -0.000000000000000000, 1.000000000000000000, -0.000000000000000000 ) ) ;
#4325 = FACE_OUTER_BOUND ( 'NONE', #206, .T. ) ;
#4326 = LINE ( 'NONE', #117, #734 ) ;
#4327 = CARTESIAN_POINT ( 'NONE',  ( 10.35533905932737930, 4.187500000000000000, -25.00000000000000000 ) ) ;
#4328 = ORIENTED_EDGE ( 'NONE', *, *, #10595, .T. ) ;
#4329 = EDGE_CURVE ( 'NONE', #492, #6119, #3341, .T. ) ;
#4330 = ORIENTED_EDGE ( 'NONE', *, *, #1610, .F. ) ;
#4331 = ORIENTED_EDGE ( 'NONE', *, *, #7205, .F. ) ;
#4332 = DIRECTION ( 'NONE',  ( -0.000000000000000000, -1.000000000000000000, -0.000000000000000000 ) ) ;
#4333 = CARTESIAN_POINT ( 'NONE',  ( -24.62111388750000174, 4.893749999044085364, -3.015216831376932151E-15 ) ) ;
#4334 = CARTESIAN_POINT ( 'NONE',  ( -17.40975659021752975, 0.7687499990440846975, -17.40975659021752975 ) ) ;
#4335 = CARTESIAN_POINT ( 'NONE',  ( -17.40975659021752975, 1.768749999044084475, -17.40975659021752975 ) ) ;
#4336 = CARTESIAN_POINT ( 'NONE',  ( -24.62111388750000174, 2.718749999044084653, -3.015216831376932151E-15 ) ) ;
#4337 = CARTESIAN_POINT ( 'NONE',  ( -17.67766952966369232, 3.237499998088169573, 17.67766952966368876 ) ) ;
#4338 = CARTESIAN_POINT ( 'NONE',  ( 0.000000000000000000, -55.00000000000000000, 0.000000000000000000 ) ) ;
#4339 = CARTESIAN_POINT ( 'NONE',  ( 0.000000000000000000, 85.00000000000000000, 0.000000000000000000 ) ) ;
#4340 = CARTESIAN_POINT ( 'NONE',  ( -1.399999999999998579, 0.000000000000000000, 0.000000000000000000 ) ) ;
#4341 = EDGE_LOOP ( 'NONE', ( #9456, #8007, #10190, #7131 ) ) ;
#4342 = ORIENTED_EDGE ( 'NONE', *, *, #5575, .F. ) ;
#4343 = EDGE_LOOP ( 'NONE', ( #2443, #10847, #9278, #9669 ) ) ;
#4344 = ORIENTED_EDGE ( 'NONE', *, *, #10386, .T. ) ;
#4345 = DIRECTION ( 'NONE',  ( 0.000000000000000000, -0.000000000000000000, 1.000000000000000000 ) ) ;
#4346 = CARTESIAN_POINT ( 'NONE',  ( 2.449293598294706414E-16, 20.00000000000000355, 2.000000000000000000 ) ) ;
#4347 = ORIENTED_EDGE ( 'NONE', *, *, #8393, .T. ) ;
#4348 = CARTESIAN_POINT ( 'NONE',  ( -7.276923788646840308, -0.001000000000001000089, -18.60400172474260216 ) ) ;
#4349 = DIRECTION ( 'NONE',  ( 1.156482317317872514E-15, 0.000000000000000000, 1.000000000000000000 ) ) ;
#4350 = DIRECTION ( 'NONE',  ( 0.000000000000000000, 0.000000000000000000, 1.000000000000000000 ) ) ;
#4351 = B_SPLINE_CURVE_WITH_KNOTS ( 'NONE', 3,
 ( #10145, #1639, #9371, #2557, #4181, #7545, #7661, #10927, #9307, #8542, #10873, #10200, #5197, #1751, #9975, #2401, #6730, #9195, #5781, #9146, #929, #1574, #8313, #7493, #2504, #3271, #6671, #2452 ),
 .UNSPECIFIED., .F., .F.,
 ( 4, 2, 2, 2, 2, 2, 2, 2, 2, 2, 2, 2, 2, 4 ),
 ( 0.000000000000000000, 0.002127673191709734957, 0.004255346383419469913, 0.008510692766838939827, 0.01063836595854867478, 0.01276603915025841147, 0.01702138553367788312, 0.01914905872538762502, 0.02127673191709736691, 0.02553207830051684377, 0.02765975149222657872, 0.02978742468393631368, 0.03191509787564604517, 0.03404277106735578012 ),
 .UNSPECIFIED. ) ;
#4352 = CARTESIAN_POINT ( 'NONE',  ( -15.60400172474251868, 25.00000000000000000, 12.47307621135349720 ) ) ;
#4353 = PLANE ( 'NONE',  #34 ) ;
#4354 = CARTESIAN_POINT ( 'NONE',  ( 17.40975659021752620, 4.268749999044084475, 17.40975659021753330 ) ) ;
#4355 = EDGE_LOOP ( 'NONE', ( #3026, #6096, #2981 ) ) ;
#4356 = EDGE_LOOP ( 'NONE', ( #4728, #608 ) ) ;
#4357 = ADVANCED_FACE ( 'NONE', ( #6796 ), #9315, .F. ) ;
#4358 = CARTESIAN_POINT ( 'NONE',  ( 3.058047309050022200, 10.00000000000000355, -6.296693311223905631 ) ) ;
#4359 = CARTESIAN_POINT ( 'NONE',  ( -17.67766952966368876, 3.987499998088168685, -17.67766952966369232 ) ) ;
#4360 = CARTESIAN_POINT ( 'NONE',  ( 10.19839929293505953, 4.581249999044083587, -24.62111388750000174 ) ) ;
#4361 = ORIENTED_EDGE ( 'NONE', *, *, #3348, .T. ) ;
#4362 = FACE_OUTER_BOUND ( 'NONE', #3845, .T. ) ;
#4363 = ITEM_DEFINED_TRANSFORMATION ( 'NONE', 'NONE', #7765,  #7040 ) ;
#4364 = DIRECTION ( 'NONE',  ( 0.000000000000000000, 0.000000000000000000, 1.000000000000000000 ) ) ;
#4365 = FACE_OUTER_BOUND ( 'NONE', #9338, .T. ) ;
#4366 = CARTESIAN_POINT ( 'NONE',  ( -24.62111388750000884, 4.781249999044083765, 10.19839929293505421 ) ) ;
#4367 = ADVANCED_FACE ( 'NONE', ( #3581 ), #1761, .F. ) ;
#4368 = MECHANICAL_DESIGN_GEOMETRIC_PRESENTATION_REPRESENTATION (  '', ( #10889 ), #10535 ) ;
#4369 = EDGE_CURVE ( 'NONE', #4450, #3067, #100, .T. ) ;
#4370 = CARTESIAN_POINT ( 'NONE',  ( -24.62111388750000174, 0.8937499990440845865, -3.015216831376932151E-15 ) ) ;
#4371 = CARTESIAN_POINT ( 'NONE',  ( 24.62111388750000174, 2.393749999044084475, 0.000000000000000000 ) ) ;
#4372 = CARTESIAN_POINT ( 'NONE',  ( -20.63749999999999574, 1.013986724829959586E-15, 6.750000000000007994 ) ) ;
#4373 = AXIS2_PLACEMENT_3D ( 'NONE', #109, #8676, #6980 ) ;
#4374 = DIRECTION ( 'NONE',  ( 0.000000000000000000, 1.000000000000000000, -0.000000000000000000 ) ) ;
#4375 = CARTESIAN_POINT ( 'NONE',  ( 17.40975659021752975, 1.518749999044084698, -17.40975659021752975 ) ) ;
#4376 = EDGE_LOOP ( 'NONE', ( #1409, #4874, #4740, #6629 ) ) ;
#4377 = DIRECTION ( 'NONE',  ( 0.000000000000000000, 0.000000000000000000, 1.000000000000000000 ) ) ;
#4378 = SURFACE_STYLE_USAGE ( .BOTH. , #4509 ) ;
#4379 = DIRECTION ( 'NONE',  ( 0.000000000000000000, 0.000000000000000000, 1.000000000000000000 ) ) ;
#4380 = CLOSED_SHELL ( 'NONE', ( #5819, #4792, #7310, #5451, #5645, #6966, #5540, #6066, #5508, #4402, #8300, #144, #2259, #1666, #3976, #8140, #5729, #5339, #1872, #2330, #8019, #5863, #9753, #628, #8569, #1883, #6678, #7600, #3265, #10809, #1826, #9898, #9827, #9437, #1802, #9909, #2814, #8162, #10752, #6732, #2059, #8709, #8758, #6536, #8613, #3620, #8464, #2737, #4094, #4527, #2726, #6521, #2586, #9633, #10442, #8085, #5657, #2759, #5921, #1001, #9597, #4240, #9450, #9497, #5446, #818, #10376, #9637, #4541, #10262, #643, #5445, #9047, #7871, #6683, #2603, #8819, #6464, #1570, #3111, #309 ) ) ;
#4381 = CARTESIAN_POINT ( 'NONE',  ( -19.39162934935757931, 5.000000000000000888, 15.17115553405142947 ) ) ;
#4382 = CARTESIAN_POINT ( 'NONE',  ( 17.67766952966368521, 2.487499998088169129, 17.67766952966369232 ) ) ;
#4383 = DIRECTION ( 'NONE',  ( -0.000000000000000000, -1.000000000000000000, -0.000000000000000000 ) ) ;
#4384 = CARTESIAN_POINT ( 'NONE',  ( 17.67766952966369232, 3.125000000000000000, -17.67766952966369232 ) ) ;
#4385 = EDGE_CURVE ( 'NONE', #9894, #4100, #4428, .T. ) ;
#4386 = EDGE_LOOP ( 'NONE', ( #4513, #8036, #2182, #8266 ) ) ;
#4387 = ORIENTED_EDGE ( 'NONE', *, *, #810, .T. ) ;
#4388 = VECTOR ( 'NONE', #2926, 1000.000000000000000 ) ;
#4389 = CARTESIAN_POINT ( 'NONE',  ( -7.171633369868158248, 7.781088913245561400, -11.42163336986839717 ) ) ;
#4390 = CARTESIAN_POINT ( 'NONE',  ( 24.62111388750000174, 2.456249999044084475, -10.19839929293505776 ) ) ;
#4391 = CARTESIAN_POINT ( 'NONE',  ( -24.62111388750000174, 0.8937499990440845865, -3.015216831376932151E-15 ) ) ;
#4392 = CARTESIAN_POINT ( 'NONE',  ( -25.00000000000000000, 5.049999998088170017, -10.35533905932738108 ) ) ;
#4393 = CARTESIAN_POINT ( 'NONE',  ( 10.19839929293506486, 5.031249999044083765, 24.62111388749999819 ) ) ;
#4394 = DIRECTION ( 'NONE',  ( 0.000000000000000000, 1.000000000000000000, 0.000000000000000000 ) ) ;
#4395 = MECHANICAL_DESIGN_GEOMETRIC_PRESENTATION_REPRESENTATION (  '', ( #8079 ), #2430 ) ;
#4396 = EDGE_CURVE ( 'NONE', #417, #915, #8518, .T. ) ;
#4397 = VERTEX_POINT ( 'NONE', #6974 ) ;
#4398 = FACE_OUTER_BOUND ( 'NONE', #9766, .T. ) ;
#4399 = CARTESIAN_POINT ( 'NONE',  ( -4.592425496802574367E-15, 4.362499998088169129, 25.00000000000000000 ) ) ;
#4400 = PLANE ( 'NONE',  #7102 ) ;
#4401 = CARTESIAN_POINT ( 'NONE',  ( 15.60400172474260927, -0.001000000000001000089, -12.47307621135339062 ) ) ;
#4402 = ADVANCED_FACE ( 'NONE', ( #4362 ), #7608, .T. ) ;
#4403 = AXIS2_PLACEMENT_3D ( 'NONE', #5057, #1675, #9467 ) ;
#4404 = CARTESIAN_POINT ( 'NONE',  ( 10.19839929293505953, 4.406249999044084653, -24.62111388750000174 ) ) ;
#4405 = DIRECTION ( 'NONE',  ( -0.8660254037844398178, 0.000000000000000000, -0.4999999999999977796 ) ) ;
#4406 = ORIENTED_EDGE ( 'NONE', *, *, #936, .T. ) ;
#4407 = VERTEX_POINT ( 'NONE', #7789 ) ;
#4408 = EDGE_LOOP ( 'NONE', ( #3394, #7087, #7392, #923, #99, #981, #10037, #5414, #3798, #4967, #730, #3927, #9688, #8830 ) ) ;
#4409 = DIRECTION ( 'NONE',  ( 0.8660254037844362651, 0.000000000000000000, -0.5000000000000042188 ) ) ;
#4410 = EDGE_CURVE ( 'NONE', #3051, #10524, #41, .T. ) ;
#4411 = DIRECTION ( 'NONE',  ( 1.000000000000000000, 0.000000000000000000, -3.491481338843131383E-15 ) ) ;
#4412 = DIRECTION ( 'NONE',  ( 0.000000000000000000, 0.000000000000000000, 1.000000000000000000 ) ) ;
#4413 = DIRECTION ( 'NONE',  ( -0.9659258262890684232, 0.2588190451025202399, 0.000000000000000000 ) ) ;
#4414 = ADVANCED_BREP_SHAPE_REPRESENTATION ( '', ( #10772, #7040 ), #8779 ) ;
#4415 = DIRECTION ( 'NONE',  ( -0.000000000000000000, -1.000000000000000000, -0.000000000000000000 ) ) ;
#4416 = DIRECTION ( 'NONE',  ( 0.000000000000000000, -1.000000000000000000, -0.000000000000000000 ) ) ;
#4417 = CARTESIAN_POINT ( 'NONE',  ( -4.592425496802574367E-15, 4.362499998088169129, 25.00000000000000000 ) ) ;
#4418 = PRODUCT_DEFINITION_FORMATION_WITH_SPECIFIED_SOURCE ( 'ANY', '', #1332, .NOT_KNOWN. ) ;
#4419 = ORIENTED_EDGE ( 'NONE', *, *, #3048, .T. ) ;
#4420 = PRODUCT ( 'Lower Catch Container', 'Lower Catch Container', '', ( #9817 ) ) ;
#4421 = CARTESIAN_POINT ( 'NONE',  ( 25.00000000000000000, 5.612499998088169129, 0.000000000000000000 ) ) ;
#4422 = DIRECTION ( 'NONE',  ( 0.000000000000000000, 0.000000000000000000, 1.000000000000000000 ) ) ;
#4423 = CARTESIAN_POINT ( 'NONE',  ( -10.19839929293505776, 4.706249999044084475, -24.62111388750000174 ) ) ;
#4424 = ORIENTED_EDGE ( 'NONE', *, *, #1390, .F. ) ;
#4425 = DIRECTION ( 'NONE',  ( 0.000000000000000000, -0.000000000000000000, 1.000000000000000000 ) ) ;
#4426 = APPLICATION_PROTOCOL_DEFINITION ( 'draft international standard', 'automotive_design', 1998, #6337 ) ;
#4427 = FACE_OUTER_BOUND ( 'NONE', #3908, .T. ) ;
#4428 = CIRCLE ( 'NONE', #10584, 2.999999999999996447 ) ;
#4429 = AXIS2_PLACEMENT_3D ( 'NONE', #4105, #3136, #6591 ) ;
#4430 = DIRECTION ( 'NONE',  ( 0.000000000000000000, 1.000000000000000000, 0.000000000000000000 ) ) ;
#4431 = CARTESIAN_POINT ( 'NONE',  ( -10.19839929293505776, 4.531249999044084653, -24.62111388750000174 ) ) ;
#4432 = PRODUCT_DEFINITION ( 'UNKNOWN', '', #1568, #4942 ) ;
#4433 = VECTOR ( 'NONE', #6115, 1000.000000000000000 ) ;
#4434 = CIRCLE ( 'NONE', #3337, 30.00000000000000000 ) ;
#4435 = APPLICATION_CONTEXT ( 'automotive_design' ) ;
#4436 = FACE_BOUND ( 'NONE', #3231, .T. ) ;
#4437 = CARTESIAN_POINT ( 'NONE',  ( -10.19839929293505776, 4.531249999044084653, -24.62111388750000174 ) ) ;
#4438 = CARTESIAN_POINT ( 'NONE',  ( 0.000000000000000000, 5.000000000000000000, 0.000000000000000000 ) ) ;
#4439 = VERTEX_POINT ( 'NONE', #5032 ) ;
#4440 = DIRECTION ( 'NONE',  ( 0.000000000000000000, 1.000000000000000000, 0.000000000000000000 ) ) ;
#4441 = SURFACE_STYLE_USAGE ( .BOTH. , #10220 ) ;
#4442 = DIRECTION ( 'NONE',  ( 0.000000000000000000, 1.000000000000000000, 0.000000000000000000 ) ) ;
#4443 = FACE_BOUND ( 'NONE', #7709, .T. ) ;
#4444 = CARTESIAN_POINT ( 'NONE',  ( -4.592425496802574367E-15, 1.362499998088169129, 25.00000000000000000 ) ) ;
#4445 = CARTESIAN_POINT ( 'NONE',  ( -17.67766952966369232, 3.625000000000000000, 17.67766952966368876 ) ) ;
#4446 = VECTOR ( 'NONE', #4416, 1000.000000000000000 ) ;
#4447 =( GEOMETRIC_REPRESENTATION_CONTEXT ( 3 ) GLOBAL_UNCERTAINTY_ASSIGNED_CONTEXT ( ( #7473 ) ) GLOBAL_UNIT_ASSIGNED_CONTEXT ( ( #2620, #8546, #7723 ) ) REPRESENTATION_CONTEXT ( 'NONE', 'WORKASPACE' ) );
#4448 =( BOUNDED_CURVE ( )  B_SPLINE_CURVE ( 2, ( #8681, #5221, #7803, #172, #3534, #9460, #1892, #237, #1126, #5763, #289, #7037, #10396, #9128, #7479, #7092, #1329, #547, #3869, #9675, #498, #9568, #2010, #6209, #7232, #6367, #2962, #5428, #2206, #3815, #4611, #394, #8060, #7967, #9725, #1375, #3711, #10608, #3020, #2150, #4760, #9623, #6421, #9772, #5385, #8841, #1282, #5533, #8896, #5584, #6309, #8943, #10450, #6264, #8115, #3928, #2099, #7144, #10503, #10553, #344, #2912, #7288, #2811, #7187, #449, #8742, #1181, #2867, #1230, #8790, #4559, #2054, #3768, #7916, #5476, #4665, #8017, #4711 ),
 .UNSPECIFIED., .F., .F. ) 
 B_SPLINE_CURVE_WITH_KNOTS ( ( 3, 2, 2, 2, 2, 2, 2, 2, 2, 2, 2, 2, 2, 2, 2, 2, 2, 2, 2, 2, 2, 2, 2, 2, 2, 2, 2, 2, 2, 2, 2, 2, 2, 2, 2, 2, 2, 2, 2, 3 ),
 ( 0.000000000000000000, 0.02500000000000000139, 0.05000000000000000278, 0.07499999999999999722, 0.1000000000000000056, 0.1250000000000000000, 0.1499999999999999944, 0.1749999999999999889, 0.2000000000000000111, 0.2250000000000000056, 0.2500000000000000000, 0.2750000000000000222, 0.2999999999999999889, 0.3250000000000000111, 0.3499999999999999778, 0.3750000000000000000, 0.4000000000000000222, 0.4249999999999999889, 0.4500000000000000111, 0.4749999999999999778, 0.5000000000000000000, 0.5250000000000000222, 0.5500000000000000444, 0.5749999999999999556, 0.5999999999999999778, 0.6250000000000000000, 0.6500000000000000222, 0.6750000000000000444, 0.6999999999999999556, 0.7249999999999999778, 0.7500000000000000000, 0.7750000000000000222, 0.8000000000000000444, 0.8249999999999999556, 0.8499999999999999778, 0.8750000000000000000, 0.9000000000000000222, 0.9250000000000000444, 0.9499999999999999556, 0.9564318172069539159 ),
 .UNSPECIFIED. ) 
 CURVE ( )  GEOMETRIC_REPRESENTATION_ITEM ( )  RATIONAL_B_SPLINE_CURVE ( ( 1.000000000000000000, 0.9238795325112867385, 1.000000000000000000, 0.9238795325112867385, 1.000000000000000000, 0.9238795325112867385, 1.000000000000000000, 0.9238795325112867385, 1.000000000000000000, 0.9238795325112867385, 1.000000000000000000, 0.9238795325112867385, 1.000000000000000000, 0.9238795325112867385, 1.000000000000000000, 0.9238795325112867385, 1.000000000000000000, 0.9238795325112867385, 1.000000000000000000, 0.9238795325112867385, 1.000000000000000000, 0.9238795325112867385, 1.000000000000000000, 0.9238795325112867385, 1.000000000000000000, 0.9238795325112867385, 1.000000000000000000, 0.9238795325112867385, 1.000000000000000000, 0.9238795325112867385, 1.000000000000000000, 0.9238795325112867385, 1.000000000000000000, 0.9238795325112867385, 1.000000000000000000, 0.9238795325112867385, 1.000000000000000000, 0.9238795325112867385, 1.000000000000000000, 0.9238795325112867385, 1.000000000000000000, 0.9238795325112867385, 1.000000000000000000, 0.9238795325112867385, 1.000000000000000000, 0.9238795325112867385, 1.000000000000000000, 0.9238795325112867385, 1.000000000000000000, 0.9238795325112867385, 1.000000000000000000, 0.9238795325112867385, 1.000000000000000000, 0.9238795325112867385, 1.000000000000000000, 0.9238795325112867385, 1.000000000000000000, 0.9238795325112867385, 1.000000000000000000, 0.9238795325112867385, 1.000000000000000000, 0.9238795325112867385, 1.000000000000000000, 0.9238795325112867385, 1.000000000000000000, 0.9238795325112867385, 1.000000000000000000, 0.9238795325112867385, 1.000000000000000000, 0.9238795325112867385, 1.000000000000000000, 0.9238795325112867385, 1.000000000000000000, 0.9238795325112867385, 1.000000000000000000, 0.9238795325112867385, 1.000000000000000000, 0.9804162826961886346, 0.9709092765868392316 ) ) 
 REPRESENTATION_ITEM ( '' )  );
#4449 = ADVANCED_FACE ( 'NONE', ( #5083 ), #876, .F. ) ;
#4450 = VERTEX_POINT ( 'NONE', #7554 ) ;
#4451 = ORIENTED_EDGE ( 'NONE', *, *, #7042, .F. ) ;
#4452 = EDGE_CURVE ( 'NONE', #7447, #2032, #2986, .T. ) ;
#4453 = CARTESIAN_POINT ( 'NONE',  ( -20.63749999999999929, 0.000000000000000000, 0.000000000000000000 ) ) ;
#4454 = CARTESIAN_POINT ( 'NONE',  ( 10.19839929293505953, 3.581249999044085364, -24.62111388750000174 ) ) ;
#4455 = CARTESIAN_POINT ( 'NONE',  ( 5.276923788646705304, 28.00000000000000000, 15.13990010960490196 ) ) ;
#4456 = CARTESIAN_POINT ( 'NONE',  ( 10.35533905932737930, 4.799999998088169129, -25.00000000000000000 ) ) ;
#4457 = CARTESIAN_POINT ( 'NONE',  ( 10.19839929293505953, 4.406249999044084653, -24.62111388750000174 ) ) ;
#4458 = AXIS2_PLACEMENT_3D ( 'NONE', #9080, #1622, #8241 ) ;
#4459 = ORIENTED_EDGE ( 'NONE', *, *, #6483, .T. ) ;
#4460 = CARTESIAN_POINT ( 'NONE',  ( 0.000000000000000000, 85.00000000000000000, -25.00000000000000000 ) ) ;
#4461 = FACE_BOUND ( 'NONE', #9727, .T. ) ;
#4462 = DIRECTION ( 'NONE',  ( 0.000000000000000000, 0.000000000000000000, 1.000000000000000000 ) ) ;
#4463 = LINE ( 'NONE', #10244, #6212 ) ;
#4464 = CARTESIAN_POINT ( 'NONE',  ( 17.40975659021752620, 5.093749999044084653, 17.40975659021753330 ) ) ;
#4465 = ADVANCED_FACE ( 'NONE', ( #326 ), #5458, .F. ) ;
#4466 = DIRECTION ( 'NONE',  ( -0.000000000000000000, 1.000000000000000000, -0.000000000000000000 ) ) ;
#4467 = ORIENTED_EDGE ( 'NONE', *, *, #2132, .F. ) ;
#4468 = VERTEX_POINT ( 'NONE', #1934 ) ;
#4469 = ORIENTED_EDGE ( 'NONE', *, *, #8601, .F. ) ;
#4470 = AXIS2_PLACEMENT_3D ( 'NONE', #10842, #1669, #9116 ) ;
#4471 = ORIENTED_EDGE ( 'NONE', *, *, #446, .F. ) ;
#4472 = FACE_OUTER_BOUND ( 'NONE', #10773, .T. ) ;
#4473 = EDGE_CURVE ( 'NONE', #7275, #9592, #5511, .T. ) ;
#4474 = AXIS2_PLACEMENT_3D ( 'NONE', #3799, #3968, #588 ) ;
#4475 = DIRECTION ( 'NONE',  ( 0.000000000000000000, 0.000000000000000000, -1.000000000000000000 ) ) ;
#4476 = EDGE_LOOP ( 'NONE', ( #3707, #10915, #3987, #4127 ) ) ;
#4477 = DIRECTION ( 'NONE',  ( 0.000000000000000000, 0.000000000000000000, -1.000000000000000000 ) ) ;
#4478 = DIRECTION ( 'NONE',  ( 0.000000000000000000, 1.000000000000000000, 0.000000000000000000 ) ) ;
#4479 = CONICAL_SURFACE ( 'NONE', #4641, 2.000000000000004441, 0.7853981633974496113 ) ;
#4480 = CARTESIAN_POINT ( 'NONE',  ( 0.000000000000000000, 28.00000000000000000, 0.000000000000000000 ) ) ;
#4481 = DIRECTION ( 'NONE',  ( -0.000000000000000000, 1.000000000000000000, -0.000000000000000000 ) ) ;
#4482 = CARTESIAN_POINT ( 'NONE',  ( -10.35533905932737575, 1.312500000000000222, -25.00000000000000000 ) ) ;
#4483 = CARTESIAN_POINT ( 'NONE',  ( -10.19839929293505776, 4.706249999044084475, -24.62111388750000174 ) ) ;
#4484 = VECTOR ( 'NONE', #205, 1000.000000000000000 ) ;
#4485 = ORIENTED_EDGE ( 'NONE', *, *, #256, .F. ) ;
#4486 = CIRCLE ( 'NONE', #6945, 6.975000000000008527 ) ;
#4487 = ORIENTED_EDGE ( 'NONE', *, *, #6647, .F. ) ;
#4488 = AXIS2_PLACEMENT_3D ( 'NONE', #9407, #1962, #7874 ) ;
#4489 = CARTESIAN_POINT ( 'NONE',  ( 17.67766952966368521, 2.875000000000000000, 17.67766952966369232 ) ) ;
#4490 = PRESENTATION_STYLE_ASSIGNMENT (( #3691 ) ) ;
#4491 = CARTESIAN_POINT ( 'NONE',  ( -4.522825247065398226E-15, 4.143749999044083587, 24.62111388750000174 ) ) ;
#4492 = ORIENTED_EDGE ( 'NONE', *, *, #7670, .T. ) ;
#4493 = VECTOR ( 'NONE', #7965, 1000.000000000000000 ) ;
#4494 = CARTESIAN_POINT ( 'NONE',  ( 0.5590169943749494497, 1.873501354054951415E-16, 6.750000000000007105 ) ) ;
#4495 = CIRCLE ( 'NONE', #8712, 24.91176187412963117 ) ;
#4496 = DIRECTION ( 'NONE',  ( 0.000000000000000000, 1.000000000000000000, 0.000000000000000000 ) ) ;
#4497 = CARTESIAN_POINT ( 'NONE',  ( -4.592425496802574367E-15, 5.362499998088169129, 25.00000000000000000 ) ) ;
#4498 = CARTESIAN_POINT ( 'NONE',  ( 5.510910596163089556E-16, 7.000000000000003553, 4.500000000000000888 ) ) ;
#4499 = AXIS2_PLACEMENT_3D ( 'NONE', #101, #2516, #7727 ) ;
#4500 = ORIENTED_EDGE ( 'NONE', *, *, #45, .T. ) ;
#4501 = AXIS2_PLACEMENT_3D ( 'NONE', #9485, #7009, #10527 ) ;
#4502 = PLANE ( 'NONE',  #2987 ) ;
#4503 = VECTOR ( 'NONE', #2613, 1000.000000000000000 ) ;
#4504 = CARTESIAN_POINT ( 'NONE',  ( 7.276923788646575630, 28.00000000000000000, -18.60400172474270875 ) ) ;
#4505 = PRODUCT_RELATED_PRODUCT_CATEGORY ( 'part', '', ( #1332 ) ) ;
#4506 = DIRECTION ( 'NONE',  ( 0.000000000000000000, 0.000000000000000000, -1.000000000000000000 ) ) ;
#4507 = ORIENTED_EDGE ( 'NONE', *, *, #8133, .F. ) ;
#4508 = FACE_OUTER_BOUND ( 'NONE', #10136, .T. ) ;
#4509 = SURFACE_SIDE_STYLE ('',( #2809 ) ) ;
#4510 = DIRECTION ( 'NONE',  ( 0.000000000000000000, 1.000000000000000000, 0.000000000000000000 ) ) ;
#4511 = PLANE ( 'NONE',  #6246 ) ;
#4512 = CARTESIAN_POINT ( 'NONE',  ( -17.67766952966368876, 0.9874999980881691286, -17.67766952966369232 ) ) ;
#4513 = ORIENTED_EDGE ( 'NONE', *, *, #4709, .F. ) ;
#4514 = ORIENTED_EDGE ( 'NONE', *, *, #1516, .T. ) ;
#4515 = ORIENTED_EDGE ( 'NONE', *, *, #9702, .T. ) ;
#4516 = CARTESIAN_POINT ( 'NONE',  ( 10.47307621135324496, 28.00000000000000000, -12.13990010960497479 ) ) ;
#4517 = CARTESIAN_POINT ( 'NONE',  ( 17.40975659021752975, 3.343749999044085097, -17.40975659021752975 ) ) ;
#4518 = CARTESIAN_POINT ( 'NONE',  ( 10.35533905932737930, 0.7999999980881692396, -25.00000000000000000 ) ) ;
#4519 = ADVANCED_FACE ( 'NONE', ( #1994 ), #10489, .F. ) ;
#4520 = CARTESIAN_POINT ( 'NONE',  ( 25.00000000000000000, 3.612499998088169129, 0.000000000000000000 ) ) ;
#4521 = CARTESIAN_POINT ( 'NONE',  ( 10.35533905932737930, 0.1874999999999999722, -25.00000000000000000 ) ) ;
#4522 =( BOUNDED_CURVE ( )  B_SPLINE_CURVE ( 2, ( #5742, #8995, #9101, #1423, #4917, #3867, #8265, #5530, #1328 ),
 .UNSPECIFIED., .F., .F. ) 
 B_SPLINE_CURVE_WITH_KNOTS ( ( 3, 2, 2, 2, 3 ),
 ( 0.3499999999999999778, 0.3750000000000000000, 0.4000000000000000222, 0.4249999999999999889, 0.4500000000000000111 ),
 .UNSPECIFIED. ) 
 CURVE ( )  GEOMETRIC_REPRESENTATION_ITEM ( )  RATIONAL_B_SPLINE_CURVE ( ( 1.000000000000000000, 0.9238795325112867385, 1.000000000000000000, 0.9238795325112867385, 1.000000000000000000, 0.9238795325112867385, 1.000000000000000000, 0.9238795325112867385, 1.000000000000000000 ) ) 
 REPRESENTATION_ITEM ( '' )  );
#4523 = CARTESIAN_POINT ( 'NONE',  ( 0.000000000000000000, 0.000000000000000000, 0.000000000000000000 ) ) ;
#4524 = DIRECTION ( 'NONE',  ( -0.000000000000000000, -1.000000000000000000, -0.000000000000000000 ) ) ;
#4525 = DIRECTION ( 'NONE',  ( 1.000000000000000000, 0.000000000000000000, -0.000000000000000000 ) ) ;
#4526 = FACE_BOUND ( 'NONE', #3531, .T. ) ;
#4527 = ADVANCED_FACE ( 'NONE', ( #7852 ), #1263, .F. ) ;
#4528 = CARTESIAN_POINT ( 'NONE',  ( 10.00000000000000000, 90.00000000000001421, 5.000000000000000000 ) ) ;
#4529 = EDGE_CURVE ( 'NONE', #10532, #2855, #3639, .T. ) ;
#4530 = ORIENTED_EDGE ( 'NONE', *, *, #130, .F. ) ;
#4531 = EDGE_LOOP ( 'NONE', ( #2723, #2908, #429, #8303 ) ) ;
#4532 = LINE ( 'NONE', #9298, #9122 ) ;
#4533 = EDGE_CURVE ( 'NONE', #3961, #10543, #9708, .T. ) ;
#4534 = CARTESIAN_POINT ( 'NONE',  ( -18.60400172474273361, -0.001000000000001000089, -7.276923788646511682 ) ) ;
#4535 = ORIENTED_EDGE ( 'NONE', *, *, #1541, .T. ) ;
#4536 = DIRECTION ( 'NONE',  ( 0.000000000000000000, 1.000000000000000000, 0.000000000000000000 ) ) ;
#4537 = DIRECTION ( 'NONE',  ( -0.4999999999999977796, -0.000000000000000000, 0.8660254037844399289 ) ) ;
#4538 = FACE_OUTER_BOUND ( 'NONE', #8724, .T. ) ;
#4539 = DIRECTION ( 'NONE',  ( 0.000000000000000000, 0.000000000000000000, 1.000000000000000000 ) ) ;
#4540 = CARTESIAN_POINT ( 'NONE',  ( 0.000000000000000000, 20.00000000000000355, 0.000000000000000000 ) ) ;
#4541 = ADVANCED_FACE ( 'NONE', ( #4547 ), #2849, .T. ) ;
#4542 = FACE_OUTER_BOUND ( 'NONE', #4355, .T. ) ;
#4543 = EDGE_LOOP ( 'NONE', ( #6622, #7204, #6247 ) ) ;
#4544 = EDGE_LOOP ( 'NONE', ( #1165, #8722, #4196, #1888 ) ) ;
#4545 = FILL_AREA_STYLE ('',( #9795 ) ) ;
#4546 = CARTESIAN_POINT ( 'NONE',  ( 10.19839929293506486, 3.206249999044084031, 24.62111388749999819 ) ) ;
#4547 = FACE_OUTER_BOUND ( 'NONE', #2930, .T. ) ;
#4548 = CARTESIAN_POINT ( 'NONE',  ( 15.74999999999999289, 28.00000000000000000, -3.000000000000055955 ) ) ;
#4549 = EDGE_CURVE ( 'NONE', #8189, #1816, #7224, .T. ) ;
#4550 = DIRECTION ( 'NONE',  ( 0.000000000000000000, 0.000000000000000000, 1.000000000000000000 ) ) ;
#4551 = ORIENTED_EDGE ( 'NONE', *, *, #1680, .F. ) ;
#4552 = CARTESIAN_POINT ( 'NONE',  ( 0.000000000000000000, 10.10000000000000497, 0.000000000000000000 ) ) ;
#4553 = CARTESIAN_POINT ( 'NONE',  ( -23.92316786293533681, 5.000000000000000000, 6.437029362807039412 ) ) ;
#4554 = CARTESIAN_POINT ( 'NONE',  ( 6.145599950363579644, 19.66631150450992038, 3.355508642977511613 ) ) ;
#4555 = EDGE_LOOP ( 'NONE', ( #9093, #524, #2548 ) ) ;
#4556 = LINE ( 'NONE', #5473, #5119 ) ;
#4557 =( NAMED_UNIT ( * ) PLANE_ANGLE_UNIT ( ) SI_UNIT ( $, .RADIAN. ) );
#4558 = CARTESIAN_POINT ( 'NONE',  ( 15.13990010960492505, 28.00000000000000000, 5.276923788646651126 ) ) ;
#4559 = CARTESIAN_POINT ( 'NONE',  ( -24.62111388750000174, 4.656249999044085541, -10.19839929293506131 ) ) ;
#4560 = DIRECTION ( 'NONE',  ( 0.000000000000000000, 0.000000000000000000, 1.000000000000000000 ) ) ;
#4561 = VERTEX_POINT ( 'NONE', #3746 ) ;
#4562 = ORIENTED_EDGE ( 'NONE', *, *, #8080, .T. ) ;
#4563 = ORIENTED_EDGE ( 'NONE', *, *, #8479, .T. ) ;
#4564 = COLOUR_RGB ( '', 0.72549020, 0.75294118, 0.79215686) ;
#4565 = CARTESIAN_POINT ( 'NONE',  ( 10.81217782649109083, 10.00000000000000355, -5.665063509461074176 ) ) ;
#4566 = CARTESIAN_POINT ( 'NONE',  ( 24.62111388749999463, 1.156249999044084431, 10.19839929293507730 ) ) ;
#4567 = CONICAL_SURFACE ( 'NONE', #2580, 25.00000000000000000, 0.3490658503988666728 ) ;
#4568 = CARTESIAN_POINT ( 'NONE',  ( 10.19839929293505953, 4.581249999044085364, -24.62111388750000174 ) ) ;
#4569 = CARTESIAN_POINT ( 'NONE',  ( -10.35533905932739174, 4.299999998088169129, 24.99999999999999289 ) ) ;
#4570 = CARTESIAN_POINT ( 'NONE',  ( 25.00000000000000000, 3.062500000000000000, -10.35533905932737753 ) ) ;
#4571 = DIRECTION ( 'NONE',  ( 0.000000000000000000, 0.000000000000000000, 1.000000000000000000 ) ) ;
#4572 = DIRECTION ( 'NONE',  ( 0.000000000000000000, 0.000000000000000000, 1.000000000000000000 ) ) ;
#4573 = CARTESIAN_POINT ( 'NONE',  ( 6.223805082245746689, 19.34316356887877930, -3.208128317448911915 ) ) ;
#4574 = DIRECTION ( 'NONE',  ( 0.8660254037844363761, 0.000000000000000000, 0.5000000000000039968 ) ) ;
#4575 = DIRECTION ( 'NONE',  ( -0.5000000000000042188, 0.000000000000000000, -0.8660254037844362651 ) ) ;
#4576 = VECTOR ( 'NONE', #8603, 1000.000000000000000 ) ;
#4577 = VECTOR ( 'NONE', #8672, 1000.000000000000000 ) ;
#4578 = ORIENTED_EDGE ( 'NONE', *, *, #5993, .T. ) ;
#4579 = EDGE_CURVE ( 'NONE', #7487, #2886, #6297, .T. ) ;
#4580 = CARTESIAN_POINT ( 'NONE',  ( 29.32100596316561081, 99.46396820659043669, -5.000000000000000000 ) ) ;
#4581 = AXIS2_PLACEMENT_3D ( 'NONE', #76, #10070, #682 ) ;
#4582 = EDGE_CURVE ( 'NONE', #9521, #9309, #9556, .T. ) ;
#4583 = VECTOR ( 'NONE', #6018, 1000.000000000000000 ) ;
#4584 = CARTESIAN_POINT ( 'NONE',  ( 9.875000000000023093, -0.001000000000001000089, 17.10400172474264835 ) ) ;
#4585 = FACE_OUTER_BOUND ( 'NONE', #9652, .T. ) ;
#4586 = CARTESIAN_POINT ( 'NONE',  ( -5.796693311223863887, 19.03096903053432598, -3.924072712834521415 ) ) ;
#4587 = DIRECTION ( 'NONE',  ( 1.000000000000000000, 0.000000000000000000, 0.000000000000000000 ) ) ;
#4588 = DIRECTION ( 'NONE',  ( 0.5000000000000009992, -0.8660254037844380415, 1.745740669421570228E-15 ) ) ;
#4589 = EDGE_CURVE ( 'NONE', #6120, #10105, #5313, .T. ) ;
#4590 = ORIENTED_EDGE ( 'NONE', *, *, #9702, .F. ) ;
#4591 = ADVANCED_FACE ( 'NONE', ( #5416 ), #8001, .F. ) ;
#4592 = AXIS2_PLACEMENT_3D ( 'NONE', #7635, #244, #903 ) ;
#4593 = VERTEX_POINT ( 'NONE', #7946 ) ;
#4594 = ADVANCED_FACE ( 'NONE', ( #8774 ), #8729, .F. ) ;
#4595 = CARTESIAN_POINT ( 'NONE',  ( 24.62111388750000174, 3.393749999044084475, 0.000000000000000000 ) ) ;
#4596 = LINE ( 'NONE', #9705, #6256 ) ;
#4597 = FACE_OUTER_BOUND ( 'NONE', #1039, .T. ) ;
#4598 = DIRECTION ( 'NONE',  ( 1.000000000000000000, 0.000000000000000000, 0.000000000000000000 ) ) ;
#4599 = DIRECTION ( 'NONE',  ( 0.000000000000000000, 0.000000000000000000, 1.000000000000000000 ) ) ;
#4600 = EDGE_CURVE ( 'NONE', #9751, #5070, #4596, .T. ) ;
#4601 = ORIENTED_EDGE ( 'NONE', *, *, #7205, .T. ) ;
#4602 = EDGE_CURVE ( 'NONE', #2139, #3676, #8000, .T. ) ;
#4603 = AXIS2_PLACEMENT_3D ( 'NONE', #2753, #6147, #5324 ) ;
#4604 = FACE_OUTER_BOUND ( 'NONE', #3789, .T. ) ;
#4605 = FACE_OUTER_BOUND ( 'NONE', #8470, .T. ) ;
#4606 = AXIS2_PLACEMENT_3D ( 'NONE', #6774, #6652, #5062 ) ;
#4607 = FACE_OUTER_BOUND ( 'NONE', #9788, .T. ) ;
#4608 = VERTEX_POINT ( 'NONE', #9501 ) ;
#4609 = CYLINDRICAL_SURFACE ( 'NONE', #1955, 2.999999999999997335 ) ;
#4610 = FACE_OUTER_BOUND ( 'NONE', #1211, .T. ) ;
#4611 = CARTESIAN_POINT ( 'NONE',  ( 17.40975659021752620, 2.093749999044084653, 17.40975659021753330 ) ) ;
#4612 = CARTESIAN_POINT ( 'NONE',  ( 5.796693311223918954, 10.00000000000000355, -3.924072712834440591 ) ) ;
#4613 = PRODUCT ( 'Inner Conical Burr Core', 'Inner Conical Burr Core', '', ( #8213 ) ) ;
#4614 = VECTOR ( 'NONE', #4973, 1000.000000000000000 ) ;
#4615 = ORIENTED_EDGE ( 'NONE', *, *, #4994, .F. ) ;
#4616 = VECTOR ( 'NONE', #3467, 1000.000000000000000 ) ;
#4617 = DIRECTION ( 'NONE',  ( 0.000000000000000000, 0.000000000000000000, 1.000000000000000000 ) ) ;
#4618 = CARTESIAN_POINT ( 'NONE',  ( -4.522825247065398226E-15, 3.968749999044084209, 24.62111388750000174 ) ) ;
#4619 = CARTESIAN_POINT ( 'NONE',  ( -10.19839929293505776, 4.706249999044086252, -24.62111388750000174 ) ) ;
#4620 = CARTESIAN_POINT ( 'NONE',  ( 10.35533905932738286, 3.812500000000000000, 24.99999999999999645 ) ) ;
#4621 = VECTOR ( 'NONE', #522, 1000.000000000000000 ) ;
#4622 = LINE ( 'NONE', #10517, #4388 ) ;
#4623 = PLANE ( 'NONE',  #5314 ) ;
#4624 = PRODUCT_DEFINITION_CONTEXT ( 'detailed design', #4435, 'design' ) ;
#4625 = CARTESIAN_POINT ( 'NONE',  ( 0.000000000000000000, 5.000000000000000000, 0.000000000000000000 ) ) ;
#4626 = CARTESIAN_POINT ( 'NONE',  ( 3.957930336368489021E-15, 25.00000000000000000, 19.75000000000000000 ) ) ;
#4627 = VERTEX_POINT ( 'NONE', #8669 ) ;
#4628 = VERTEX_POINT ( 'NONE', #1112 ) ;
#4629 = AXIS2_PLACEMENT_3D ( 'NONE', #9794, #7019, #215 ) ;
#4630 = CIRCLE ( 'NONE', #3549, 4.999999999999997335 ) ;
#4631 = DIRECTION ( 'NONE',  ( 0.000000000000000000, 1.000000000000000000, 0.000000000000000000 ) ) ;
#4632 = ORIENTED_EDGE ( 'NONE', *, *, #7486, .T. ) ;
#4633 = CARTESIAN_POINT ( 'NONE',  ( 1.500000000000000000, 88.00000000000001421, 1.500000000000000000 ) ) ;
#4634 = LINE ( 'NONE', #7989, #1104 ) ;
#4635 = CARTESIAN_POINT ( 'NONE',  ( 0.4330127018922190207, 0.000000000000000000, 0.2500000000000004996 ) ) ;
#4636 = DIRECTION ( 'NONE',  ( -0.000000000000000000, 1.000000000000000000, -0.000000000000000000 ) ) ;
#4637 = CIRCLE ( 'NONE', #10794, 3.379762621896238883 ) ;
#4638 = ORIENTED_EDGE ( 'NONE', *, *, #520, .T. ) ;
#4639 = VECTOR ( 'NONE', #2635, 1000.000000000000000 ) ;
#4640 = VERTEX_POINT ( 'NONE', #4494 ) ;
#4641 = AXIS2_PLACEMENT_3D ( 'NONE', #8596, #1207, #8767 ) ;
#4642 = EDGE_CURVE ( 'NONE', #10846, #5785, #10745, .T. ) ;
#4643 = PLANE ( 'NONE',  #7981 ) ;
#4644 = EDGE_CURVE ( 'NONE', #292, #39, #9656, .T. ) ;
#4645 = DIRECTION ( 'NONE',  ( 0.000000000000000000, 1.000000000000000000, 0.000000000000000000 ) ) ;
#4646 = DIRECTION ( 'NONE',  ( 0.000000000000000000, 0.000000000000000000, 1.000000000000000000 ) ) ;
#4647 = DIRECTION ( 'NONE',  ( 0.000000000000000000, 0.000000000000000000, 1.000000000000000000 ) ) ;
#4648 = DIRECTION ( 'NONE',  ( 1.000000000000000000, 0.000000000000000000, 0.000000000000000000 ) ) ;
#4649 = VECTOR ( 'NONE', #8821, 1000.000000000000114 ) ;
#4650 = CIRCLE ( 'NONE', #5694, 25.00000000000000000 ) ;
#4651 = ADVANCED_FACE ( 'NONE', ( #4901 ), #5376, .T. ) ;
#4652 = VECTOR ( 'NONE', #4636, 1000.000000000000000 ) ;
#4653 = ORIENTED_EDGE ( 'NONE', *, *, #6507, .T. ) ;
#4654 = CIRCLE ( 'NONE', #3200, 2.999999999999996447 ) ;
#4655 = AXIS2_PLACEMENT_3D ( 'NONE', #2692, #6025, #5085 ) ;
#4656 = CARTESIAN_POINT ( 'NONE',  ( 2.500000000000000444, 1.000000000000001998, 0.5773502691896277295 ) ) ;
#4657 = CARTESIAN_POINT ( 'NONE',  ( 3.058047309050022200, 19.03096903053434019, -6.296693311223905631 ) ) ;
#4658 = CARTESIAN_POINT ( 'NONE',  ( -10.19839929293505776, 2.706249999044084475, -24.62111388750000174 ) ) ;
#4659 = VERTEX_POINT ( 'NONE', #3159 ) ;
#4660 = ADVANCED_FACE ( 'NONE', ( #9804 ), #9041, .F. ) ;
#4661 = LINE ( 'NONE', #9722, #6522 ) ;
#4662 = PRESENTATION_STYLE_ASSIGNMENT (( #3812 ) ) ;
#4663 = LINE ( 'NONE', #2960, #2874 ) ;
#4664 = EDGE_LOOP ( 'NONE', ( #10122, #579, #7471, #123 ) ) ;
#4665 = CARTESIAN_POINT ( 'NONE',  ( -4.522825247065398226E-15, 4.968749999044083765, 24.62111388750000174 ) ) ;
#4666 = LINE ( 'NONE', #3712, #5620 ) ;
#4667 = ORIENTED_EDGE ( 'NONE', *, *, #396, .F. ) ;
#4668 = AXIS2_PLACEMENT_3D ( 'NONE', #1042, #4415, #209 ) ;
#4669 = EDGE_CURVE ( 'NONE', #4407, #7330, #6613, .T. ) ;
#4670 = ORIENTED_EDGE ( 'NONE', *, *, #7885, .F. ) ;
#4671 = EDGE_LOOP ( 'NONE', ( #8837, #1106, #745, #8110 ) ) ;
#4672 = CIRCLE ( 'NONE', #10828, 5.000000000000000000 ) ;
#4673 = DIRECTION ( 'NONE',  ( 0.9659258262890684232, -0.2588190451025202399, 0.000000000000000000 ) ) ;
#4674 = CARTESIAN_POINT ( 'NONE',  ( -10.19839929293505776, 3.531249999044084653, -24.62111388750000174 ) ) ;
#4675 = CARTESIAN_POINT ( 'NONE',  ( 10.19839929293506486, 4.206249999044085364, 24.62111388749999819 ) ) ;
#4676 = EDGE_LOOP ( 'NONE', ( #841, #5671, #5845, #6214 ) ) ;
#4677 = AXIS2_PLACEMENT_3D ( 'NONE', #10800, #8194, #6444 ) ;
#4678 = CARTESIAN_POINT ( 'NONE',  ( -17.67766952966368876, 3.375000000000000000, -17.67766952966369232 ) ) ;
#4679 = CARTESIAN_POINT ( 'NONE',  ( -4.592425496802574367E-15, 1.362499998088169129, 25.00000000000000000 ) ) ;
#4680 = CARTESIAN_POINT ( 'NONE',  ( 82.32050807568876394, 0.000000000000000000, -5.000000000000000000 ) ) ;
#4681 = CARTESIAN_POINT ( 'NONE',  ( -4.592425496802574367E-15, 0.7500000000000000000, 25.00000000000000000 ) ) ;
#4682 = EDGE_CURVE ( 'NONE', #1319, #375, #6556, .T. ) ;
#4683 = CARTESIAN_POINT ( 'NONE',  ( 10.35533905932737930, 2.187500000000000444, -25.00000000000000000 ) ) ;
#4684 = ORIENTED_EDGE ( 'NONE', *, *, #525, .T. ) ;
#4685 = ORIENTED_EDGE ( 'NONE', *, *, #9364, .T. ) ;
#4686 = ORIENTED_EDGE ( 'NONE', *, *, #5257, .T. ) ;
#4687 = ORIENTED_EDGE ( 'NONE', *, *, #4579, .T. ) ;
#4688 = FACE_OUTER_BOUND ( 'NONE', #6674, .T. ) ;
#4689 = DIRECTION ( 'NONE',  ( 0.000000000000000000, -0.000000000000000000, 1.000000000000000000 ) ) ;
#4690 = CYLINDRICAL_SURFACE ( 'NONE', #6082, 2.999999999999997780 ) ;
#4691 = CARTESIAN_POINT ( 'NONE',  ( 6.062177826491051746, 20.00000000000000355, 3.500000000000027089 ) ) ;
#4692 = FACE_OUTER_BOUND ( 'NONE', #10534, .T. ) ;
#4693 = CARTESIAN_POINT ( 'NONE',  ( 0.000000000000000000, 25.00000000000000355, 0.000000000000000000 ) ) ;
#4694 = EDGE_LOOP ( 'NONE', ( #200, #1493, #8368 ) ) ;
#4695 = EDGE_LOOP ( 'NONE', ( #3439, #2474, #8037, #131 ) ) ;
#4696 = EDGE_LOOP ( 'NONE', ( #6553, #1074, #732 ) ) ;
#4697 = DIRECTION ( 'NONE',  ( 0.000000000000000000, 0.000000000000000000, -1.000000000000000000 ) ) ;
#4698 = DIRECTION ( 'NONE',  ( -1.000000000000000000, 0.000000000000000000, 0.000000000000000000 ) ) ;
#4699 = DIRECTION ( 'NONE',  ( 0.000000000000000000, 1.000000000000000000, 0.000000000000000000 ) ) ;
#4700 = CARTESIAN_POINT ( 'NONE',  ( -3.058047309049933382, 19.03096903053431532, -6.296693311223948264 ) ) ;
#4701 = DIRECTION ( 'NONE',  ( 1.000000000000000000, 0.000000000000000000, -1.069128445102650095E-14 ) ) ;
#4702 = EDGE_CURVE ( 'NONE', #1515, #7572, #10589, .T. ) ;
#4703 = ORIENTED_EDGE ( 'NONE', *, *, #10240, .F. ) ;
#4704 = DIRECTION ( 'NONE',  ( 0.000000000000000000, 2.775557561562887961E-17, 1.000000000000000000 ) ) ;
#4705 = DIRECTION ( 'NONE',  ( 0.000000000000000000, 0.000000000000000000, 1.000000000000000000 ) ) ;
#4706 = CARTESIAN_POINT ( 'NONE',  ( 24.62111388750000174, 3.393749999044084475, 0.000000000000000000 ) ) ;
#4707 = EDGE_LOOP ( 'NONE', ( #3503, #3888, #2090, #5456 ) ) ;
#4708 = CARTESIAN_POINT ( 'NONE',  ( -12.13990010960501031, 25.00000000000000000, -10.47307621135320410 ) ) ;
#4709 = EDGE_CURVE ( 'NONE', #4627, #4897, #4072, .T. ) ;
#4710 = FACE_OUTER_BOUND ( 'NONE', #6173, .T. ) ;
#4711 = CARTESIAN_POINT ( 'NONE',  ( 4.895565917430008795, 5.000000000000001776, 24.12949820052922334 ) ) ;
#4712 = CARTESIAN_POINT ( 'NONE',  ( 1.530808498934191521E-15, 4.250000000000000000, -25.00000000000000000 ) ) ;
#4713 = EDGE_LOOP ( 'NONE', ( #5573, #8193 ) ) ;
#4714 = EDGE_CURVE ( 'NONE', #2942, #10165, #427, .T. ) ;
#4715 = EDGE_LOOP ( 'NONE', ( #4285, #4868 ) ) ;
#4716 = ADVANCED_FACE ( 'NONE', ( #9757 ), #8202, .T. ) ;
#4717 = CARTESIAN_POINT ( 'NONE',  ( -24.62111388750000174, 2.718749999044084653, -3.015216831376932151E-15 ) ) ;
#4718 = CARTESIAN_POINT ( 'NONE',  ( 17.40975659021752620, 1.268749999044084698, 17.40975659021753330 ) ) ;
#4719 = ORIENTED_EDGE ( 'NONE', *, *, #2274, .T. ) ;
#4720 = CARTESIAN_POINT ( 'NONE',  ( -10.35533905932739174, 3.687500000000000444, 24.99999999999999289 ) ) ;
#4721 = EDGE_CURVE ( 'NONE', #5726, #8379, #6454, .T. ) ;
#4722 = FACE_OUTER_BOUND ( 'NONE', #4664, .T. ) ;
#4723 = CARTESIAN_POINT ( 'NONE',  ( -20.63749999999999574, -1.873501354054951662E-16, -6.750000000000007994 ) ) ;
#4724 = DIRECTION ( 'NONE',  ( 0.4999999999999949485, 0.000000000000000000, 0.8660254037844415942 ) ) ;
#4725 = CARTESIAN_POINT ( 'NONE',  ( 5.937177826491071286, 19.75000000000000000, -2.850480947161653233 ) ) ;
#4726 = CARTESIAN_POINT ( 'NONE',  ( -25.00000000000001421, 2.562500000000000444, 10.35533905932737397 ) ) ;
#4727 =( GEOMETRIC_REPRESENTATION_CONTEXT ( 3 ) GLOBAL_UNCERTAINTY_ASSIGNED_CONTEXT ( ( #8138 ) ) GLOBAL_UNIT_ASSIGNED_CONTEXT ( ( #2638, #9458, #1948 ) ) REPRESENTATION_CONTEXT ( 'NONE', 'WORKASPACE' ) );
#4728 = ORIENTED_EDGE ( 'NONE', *, *, #8877, .T. ) ;
#4729 = ORIENTED_EDGE ( 'NONE', *, *, #10313, .F. ) ;
#4730 = ADVANCED_FACE ( 'NONE', ( #3002 ), #9088, .T. ) ;
#4731 = CARTESIAN_POINT ( 'NONE',  ( -25.00000000000000000, 4.500000000000000888, -3.061616997868383043E-15 ) ) ;
#4732 = DIRECTION ( 'NONE',  ( 1.000000000000000000, -0.000000000000000000, 1.224646799147353207E-16 ) ) ;
#4733 = EDGE_CURVE ( 'NONE', #9084, #620, #9775, .T. ) ;
#4734 = VECTOR ( 'NONE', #10823, 1000.000000000000000 ) ;
#4735 = SURFACE_STYLE_USAGE ( .BOTH. , #6638 ) ;
#4736 = DIRECTION ( 'NONE',  ( -0.000000000000000000, 1.000000000000000000, -0.000000000000000000 ) ) ;
#4737 = DIRECTION ( 'NONE',  ( -0.5000000000000069944, 0.000000000000000000, 0.8660254037844344888 ) ) ;
#4738 = CARTESIAN_POINT ( 'NONE',  ( 0.000000000000000000, 10.00000000000000355, 0.000000000000000000 ) ) ;
#4739 = CARTESIAN_POINT ( 'NONE',  ( -6.982120021884473005, 10.00000000000000355, 0.4999999999999268363 ) ) ;
#4740 = ORIENTED_EDGE ( 'NONE', *, *, #7594, .F. ) ;
#4741 = MECHANICAL_DESIGN_GEOMETRIC_PRESENTATION_REPRESENTATION (  '', ( #9679 ), #4197 ) ;
#4742 = VERTEX_POINT ( 'NONE', #3104 ) ;
#4743 = EDGE_CURVE ( 'NONE', #10892, #8014, #589, .T. ) ;
#4744 = VECTOR ( 'NONE', #5173, 1000.000000000000000 ) ;
#4745 = DIRECTION ( 'NONE',  ( -0.8660254037844327124, 0.000000000000000000, 0.5000000000000103251 ) ) ;
#4746 = DIRECTION ( 'NONE',  ( -1.000000000000000000, 0.000000000000000000, 0.000000000000000000 ) ) ;
#4747 = DIRECTION ( 'NONE',  ( 0.000000000000000000, -1.000000000000000000, 0.000000000000000000 ) ) ;
#4748 = DIRECTION ( 'NONE',  ( 0.000000000000000000, 1.000000000000000000, 0.000000000000000000 ) ) ;
#4749 = CARTESIAN_POINT ( 'NONE',  ( 3.223142256880076948E-15, 28.00000000000000000, 15.75000000000000000 ) ) ;
#4750 = CIRCLE ( 'NONE', #7558, 6.999999999999997335 ) ;
#4751 = ORIENTED_EDGE ( 'NONE', *, *, #9507, .T. ) ;
#4752 = ORIENTED_EDGE ( 'NONE', *, *, #268, .T. ) ;
#4753 = DIRECTION ( 'NONE',  ( 0.000000000000000000, -0.8660254037844380415, 0.5000000000000009992 ) ) ;
#4754 = CARTESIAN_POINT ( 'NONE',  ( 10.19839929293506486, 3.206249999044084031, 24.62111388749999819 ) ) ;
#4755 = ORIENTED_EDGE ( 'NONE', *, *, #3823, .F. ) ;
#4756 = CARTESIAN_POINT ( 'NONE',  ( 15.60400172474260927, 25.00000000000000000, -12.47307621135339062 ) ) ;
#4757 = SHAPE_REPRESENTATION_RELATIONSHIP ( 'NONE' , 'NONE' ,  #9997, #4414 ) ;
#4758 = DIRECTION ( 'NONE',  ( -0.000000000000000000, -0.8660254037844380415, -0.5000000000000009992 ) ) ;
#4759 = EDGE_LOOP ( 'NONE', ( #1285, #7365, #6780, #1722 ) ) ;
#4760 = CARTESIAN_POINT ( 'NONE',  ( -24.62111388750000174, 2.718749999044084653, -3.015216831376932151E-15 ) ) ;
#4761 = CARTESIAN_POINT ( 'NONE',  ( 1.530808498934191521E-15, 2.862499998088169573, -25.00000000000000000 ) ) ;
#4762 = ORIENTED_EDGE ( 'NONE', *, *, #5039, .F. ) ;
#4763 = ORIENTED_EDGE ( 'NONE', *, *, #3333, .F. ) ;
#4764 = VERTEX_POINT ( 'NONE', #9972 ) ;
#4765 = AXIS2_PLACEMENT_3D ( 'NONE', #4264, #9226, #1607 ) ;
#4766 = CARTESIAN_POINT ( 'NONE',  ( 17.67766952966368521, 3.487499998088169129, 17.67766952966369232 ) ) ;
#4767 = CARTESIAN_POINT ( 'NONE',  ( -20.63749999999999574, 0.000000000000000000, 0.000000000000000000 ) ) ;
#4768 = CARTESIAN_POINT ( 'NONE',  ( 17.40975659021752975, 2.518749999044084475, -17.40975659021752975 ) ) ;
#4769 = CARTESIAN_POINT ( 'NONE',  ( 17.67766952966369232, 3.125000000000000000, -17.67766952966369232 ) ) ;
#4770 = EDGE_CURVE ( 'NONE', #10229, #5566, #334, .T. ) ;
#4771 = EDGE_CURVE ( 'NONE', #6537, #8862, #6965, .T. ) ;
#4772 = CARTESIAN_POINT ( 'NONE',  ( -3.223142256880076948E-15, -0.001000000000001000089, -15.75000000000000000 ) ) ;
#4773 = DIRECTION ( 'NONE',  ( -0.8660254037844328234, 0.000000000000000000, 0.5000000000000098810 ) ) ;
#4774 = LINE ( 'NONE', #2270, #3913 ) ;
#4775 = PLANE ( 'NONE',  #4230 ) ;
#4776 = AXIS2_PLACEMENT_3D ( 'NONE', #545, #3279, #10038 ) ;
#4777 = AXIS2_PLACEMENT_3D ( 'NONE', #7678, #7797, #8616 ) ;
#4778 = ORIENTED_EDGE ( 'NONE', *, *, #1516, .F. ) ;
#4779 = ORIENTED_EDGE ( 'NONE', *, *, #2571, .T. ) ;
#4780 = EDGE_LOOP ( 'NONE', ( #8114, #6630 ) ) ;
#4781 = EDGE_CURVE ( 'NONE', #7939, #7899, #8372, .T. ) ;
#4782 = ORIENTED_EDGE ( 'NONE', *, *, #10369, .T. ) ;
#4783 = DIRECTION ( 'NONE',  ( 0.000000000000000000, 0.000000000000000000, -1.000000000000000000 ) ) ;
#4784 = CIRCLE ( 'NONE', #201, 5.999999999999999112 ) ;
#4785 = COLOUR_RGB ( '', 0.09019608, 0.27058824, 0.51372549) ;
#4786 = DIRECTION ( 'NONE',  ( 0.000000000000000000, 0.9230769230769232392, 0.3846153846153844702 ) ) ;
#4787 =( LENGTH_UNIT ( ) NAMED_UNIT ( * ) SI_UNIT ( .MILLI., .METRE. ) );
#4788 = EDGE_CURVE ( 'NONE', #10138, #6596, #1746, .T. ) ;
#4789 = DIRECTION ( 'NONE',  ( 1.000000000000000000, 0.000000000000000000, 0.000000000000000000 ) ) ;
#4790 = DIRECTION ( 'NONE',  ( 0.000000000000000000, 1.000000000000000000, 0.000000000000000000 ) ) ;
#4791 = CYLINDRICAL_SURFACE ( 'NONE', #6574, 6.999999999999997335 ) ;
#4792 = ADVANCED_FACE ( 'NONE', ( #10923 ), #1636, .F. ) ;
#4793 = VECTOR ( 'NONE', #4026, 1000.000000000000000 ) ;
#4794 =( BOUNDED_CURVE ( )  B_SPLINE_CURVE ( 3, ( #925, #7658, #89, #10197 ),
 .UNSPECIFIED., .F., .F. ) 
 B_SPLINE_CURVE_WITH_KNOTS ( ( 4, 4 ),
 ( 3.927175151554405996, 3.998664601439927413 ),
 .UNSPECIFIED. ) 
 CURVE ( )  GEOMETRIC_REPRESENTATION_ITEM ( )  RATIONAL_B_SPLINE_CURVE ( ( 1.000000000000000000, 0.9995741502243209453, 0.9995741502243209453, 1.000000000000000000 ) ) 
 REPRESENTATION_ITEM ( '' )  );
#4795 = ORIENTED_EDGE ( 'NONE', *, *, #5590, .F. ) ;
#4796 = EDGE_CURVE ( 'NONE', #9663, #10596, #9366, .T. ) ;
#4797 = VERTEX_POINT ( 'NONE', #2612 ) ;
#4798 = VERTEX_POINT ( 'NONE', #5023 ) ;
#4799 = DIRECTION ( 'NONE',  ( 0.000000000000000000, -1.000000000000000000, 2.775557561562888270E-17 ) ) ;
#4800 = DIRECTION ( 'NONE',  ( 0.000000000000000000, 0.000000000000000000, 1.000000000000000000 ) ) ;
#4801 = DIRECTION ( 'NONE',  ( 0.000000000000000000, 0.000000000000000000, 1.000000000000000000 ) ) ;
#4802 = AXIS2_PLACEMENT_3D ( 'NONE', #8465, #10801, #3373 ) ;
#4803 = DIRECTION ( 'NONE',  ( 1.000000000000000000, 0.000000000000000000, 0.000000000000000000 ) ) ;
#4804 = PLANE ( 'NONE',  #4989 ) ;
#4805 = ORIENTED_EDGE ( 'NONE', *, *, #7904, .T. ) ;
#4806 = ORIENTED_EDGE ( 'NONE', *, *, #307, .F. ) ;
#4807 = AXIS2_PLACEMENT_3D ( 'NONE', #1343, #8077, #511 ) ;
#4808 = DIRECTION ( 'NONE',  ( 1.000000000000000000, 0.000000000000000000, 0.000000000000000000 ) ) ;
#4809 = DIRECTION ( 'NONE',  ( -0.5000000000000073275, 0.000000000000000000, -0.8660254037844344888 ) ) ;
#4810 = CARTESIAN_POINT ( 'NONE',  ( -24.62111388750000174, 2.831249999044084475, -10.19839929293506131 ) ) ;
#4811 = EDGE_LOOP ( 'NONE', ( #7794, #5696, #1859, #7783, #6841 ) ) ;
#4812 = AXIS2_PLACEMENT_3D ( 'NONE', #7669, #2405, #10150 ) ;
#4813 = DIRECTION ( 'NONE',  ( 0.000000000000000000, 0.000000000000000000, -1.000000000000000000 ) ) ;
#4814 = CARTESIAN_POINT ( 'NONE',  ( 2.500000000000000444, 1.000000000000001998, 0.5773502691896277295 ) ) ;
#4815 = CARTESIAN_POINT ( 'NONE',  ( 1.530808498934191521E-15, 1.250000000000000000, -25.00000000000000000 ) ) ;
#4816 = CARTESIAN_POINT ( 'NONE',  ( -17.40975659021753330, 2.843749999044085097, 17.40975659021752975 ) ) ;
#4817 = CIRCLE ( 'NONE', #2491, 0.7499999999999997780 ) ;
#4818 = ADVANCED_FACE ( 'NONE', ( #88 ), #7596, .F. ) ;
#4819 = EDGE_LOOP ( 'NONE', ( #7719, #3805, #4143, #10656 ) ) ;
#4820 = ORIENTED_EDGE ( 'NONE', *, *, #5121, .F. ) ;
#4821 = AXIS2_PLACEMENT_3D ( 'NONE', #5297, #1097, #4475 ) ;
#4822 = ORIENTED_EDGE ( 'NONE', *, *, #2585, .F. ) ;
#4823 = CARTESIAN_POINT ( 'NONE',  ( 10.35533905932738286, 3.424999998088169573, 24.99999999999999645 ) ) ;
#4824 = DIRECTION ( 'NONE',  ( 0.000000000000000000, 0.000000000000000000, 1.000000000000000000 ) ) ;
#4825 = AXIS2_PLACEMENT_3D ( 'NONE', #10074, #5940, #5888 ) ;
#4826 = CARTESIAN_POINT ( 'NONE',  ( 17.40975659021752975, 1.343749999044084653, -17.40975659021752975 ) ) ;
#4827 = ORIENTED_EDGE ( 'NONE', *, *, #4771, .F. ) ;
#4828 = DIRECTION ( 'NONE',  ( 0.000000000000000000, 0.000000000000000000, -1.000000000000000000 ) ) ;
#4829 = SHAPE_REPRESENTATION_RELATIONSHIP ( 'NONE' , 'NONE' ,  #5021, #715 ) ;
#4830 = CARTESIAN_POINT ( 'NONE',  ( 1.500000000000001776, -1.415534356397074737E-16, -5.100000000000006750 ) ) ;
#4831 = AXIS2_PLACEMENT_3D ( 'NONE', #2936, #4631, #6339 ) ;
#4832 = CARTESIAN_POINT ( 'NONE',  ( 24.99999999999999289, 1.549999998088169129, 10.35533905932739529 ) ) ;
#4833 = DIRECTION ( 'NONE',  ( -1.000000000000000000, 0.000000000000000000, 0.000000000000000000 ) ) ;
#4834 = AXIS2_PLACEMENT_3D ( 'NONE', #9043, #7271, #10747 ) ;
#4835 = CARTESIAN_POINT ( 'NONE',  ( 87.32050807568876394, 89.28203230275514102, 0.000000000000000000 ) ) ;
#4836 = CIRCLE ( 'NONE', #5201, 4.999999999999987566 ) ;
#4837 = ORIENTED_EDGE ( 'NONE', *, *, #1584, .F. ) ;
#4838 = VERTEX_POINT ( 'NONE', #4178 ) ;
#4839 = ORIENTED_EDGE ( 'NONE', *, *, #10770, .T. ) ;
#4840 = ORIENTED_EDGE ( 'NONE', *, *, #5121, .T. ) ;
#4841 = EDGE_CURVE ( 'NONE', #10217, #9174, #4010, .T. ) ;
#4842 = VECTOR ( 'NONE', #1411, 1000.000000000000000 ) ;
#4843 = UNCERTAINTY_MEASURE_WITH_UNIT (LENGTH_MEASURE( 1.000000000000000082E-05 ), #1730, 'distance_accuracy_value', 'NONE');
#4844 = VECTOR ( 'NONE', #9431, 1000.000000000000114 ) ;
#4845 = EDGE_LOOP ( 'NONE', ( #6814, #2402, #5604, #33 ) ) ;
#4846 = CARTESIAN_POINT ( 'NONE',  ( 0.000000000000000000, 31.00000000000000000, 0.000000000000000000 ) ) ;
#4847 = ADVANCED_FACE ( 'NONE', ( #6785 ), #10870, .F. ) ;
#4848 = CARTESIAN_POINT ( 'NONE',  ( 1.500000000000000000, 83.00000000000000000, 1.500000000000000000 ) ) ;
#4849 = CARTESIAN_POINT ( 'NONE',  ( -10.19839929293507552, 1.906249999044084431, 24.62111388749999463 ) ) ;
#4850 = FACE_OUTER_BOUND ( 'NONE', #3079, .T. ) ;
#4851 = ORIENTED_EDGE ( 'NONE', *, *, #6336, .F. ) ;
#4852 = EDGE_CURVE ( 'NONE', #10741, #1857, #9409, .T. ) ;
#4853 = APPLICATION_CONTEXT ( 'automotive_design' ) ;
#4854 = EDGE_LOOP ( 'NONE', ( #9018, #1910, #6041, #9478 ) ) ;
#4855 = CARTESIAN_POINT ( 'NONE',  ( -20.63749999999999574, 0.000000000000000000, 0.000000000000000000 ) ) ;
#4856 = CARTESIAN_POINT ( 'NONE',  ( 0.000000000000000000, 0.000000000000000000, 0.000000000000000000 ) ) ;
#4857 = EDGE_CURVE ( 'NONE', #9230, #1424, #10917, .T. ) ;
#4858 = DIRECTION ( 'NONE',  ( -0.000000000000000000, -1.000000000000000000, -0.000000000000000000 ) ) ;
#4859 =( BOUNDED_CURVE ( )  B_SPLINE_CURVE ( 2, ( #8693, #1139, #126, #4518, #10235 ),
 .UNSPECIFIED., .F., .F. ) 
 B_SPLINE_CURVE_WITH_KNOTS ( ( 3, 2, 3 ),
 ( 0.000000000000000000, 0.02500000000000000486, 0.05000000000000000971 ),
 .UNSPECIFIED. ) 
 CURVE ( )  GEOMETRIC_REPRESENTATION_ITEM ( )  RATIONAL_B_SPLINE_CURVE ( ( 1.000000000000000000, 0.9238795325112867385, 1.000000000000000000, 0.9238795325112867385, 1.000000000000000000 ) ) 
 REPRESENTATION_ITEM ( '' )  );
#4860 = CARTESIAN_POINT ( 'NONE',  ( 10.35533905932734733, 4.187500000000000888, -25.00000000000004263 ) ) ;
#4861 = CARTESIAN_POINT ( 'NONE',  ( 0.000000000000000000, 27.99999999999999645, -25.00000000000000000 ) ) ;
#4862 = VERTEX_POINT ( 'NONE', #3267 ) ;
#4863 = ORIENTED_EDGE ( 'NONE', *, *, #7668, .T. ) ;
#4864 = DIRECTION ( 'NONE',  ( 0.000000000000000000, 1.000000000000000000, 0.000000000000000000 ) ) ;
#4865 = DIRECTION ( 'NONE',  ( -0.000000000000000000, -0.000000000000000000, -1.000000000000000000 ) ) ;
#4866 = CARTESIAN_POINT ( 'NONE',  ( -10.19839929293507375, 3.081249999044084920, 24.62111388749999108 ) ) ;
#4867 = ADVANCED_FACE ( 'NONE', ( #3445 ), #5193, .T. ) ;
#4868 = ORIENTED_EDGE ( 'NONE', *, *, #7734, .F. ) ;
#4869 = CARTESIAN_POINT ( 'NONE',  ( 67.97877056362573001, 89.28203230275514102, 5.000000000000000000 ) ) ;
#4870 = DIRECTION ( 'NONE',  ( -1.000000000000000000, 0.000000000000000000, -7.228014483236695816E-17 ) ) ;
#4871 = DIRECTION ( 'NONE',  ( 0.000000000000000000, -2.775557561562887961E-17, -1.000000000000000000 ) ) ;
#4872 = CARTESIAN_POINT ( 'NONE',  ( 17.40975659021752975, 0.3437499990440845421, -17.40975659021752975 ) ) ;
#4873 = VERTEX_POINT ( 'NONE', #1806 ) ;
#4874 = ORIENTED_EDGE ( 'NONE', *, *, #1270, .F. ) ;
#4875 = CARTESIAN_POINT ( 'NONE',  ( 25.00000000000000000, 4.612499998088169129, 0.000000000000000000 ) ) ;
#4876 = CARTESIAN_POINT ( 'NONE',  ( -1.500000000000000444, 83.00000000000000000, -1.500000000000000222 ) ) ;
#4877 = CARTESIAN_POINT ( 'NONE',  ( -10.19839929293505776, 0.5312499990440845421, -24.62111388750000174 ) ) ;
#4878 = ORIENTED_EDGE ( 'NONE', *, *, #7668, .F. ) ;
#4879 = DIRECTION ( 'NONE',  ( 0.4330127018922172444, 0.8660254037844380415, 0.2500000000000055511 ) ) ;
#4880 = CARTESIAN_POINT ( 'NONE',  ( -6.296693311223874545, 19.03096903053432598, -3.058047309050087925 ) ) ;
#4881 = CARTESIAN_POINT ( 'NONE',  ( 0.000000000000000000, 20.00000000000000355, 0.000000000000000000 ) ) ;
#4882 = DIRECTION ( 'NONE',  ( 0.000000000000000000, 0.000000000000000000, 1.000000000000000000 ) ) ;
#4883 = LINE ( 'NONE', #9071, #2832 ) ;
#4884 = EDGE_LOOP ( 'NONE', ( #6331, #9808, #7708, #4535 ) ) ;
#4885 = EDGE_LOOP ( 'NONE', ( #1002, #3850, #6301, #4752 ) ) ;
#4886 = CARTESIAN_POINT ( 'NONE',  ( 24.62111388750000174, 2.218749999044084653, 0.000000000000000000 ) ) ;
#4887 = CARTESIAN_POINT ( 'NONE',  ( 0.000000000000000000, 1.734723475976807094E-16, 6.250000000000007105 ) ) ;
#4888 = CARTESIAN_POINT ( 'NONE',  ( -17.99166497301935408, 4.999999999999999112, 16.96057692830995478 ) ) ;
#4889 = DIRECTION ( 'NONE',  ( 0.000000000000000000, 1.000000000000000000, 0.000000000000000000 ) ) ;
#4890 = DIRECTION ( 'NONE',  ( -0.000000000000000000, 1.000000000000000000, -0.000000000000000000 ) ) ;
#4891 = CARTESIAN_POINT ( 'NONE',  ( -24.62111388750000174, 1.656249999044084431, -10.19839929293506131 ) ) ;
#4892 = CARTESIAN_POINT ( 'NONE',  ( 0.000000000000000000, 10.00000000000000355, 0.000000000000000000 ) ) ;
#4893 = ORIENTED_EDGE ( 'NONE', *, *, #5065, .T. ) ;
#4894 = VERTEX_POINT ( 'NONE', #6070 ) ;
#4895 = ORIENTED_EDGE ( 'NONE', *, *, #1336, .T. ) ;
#4896 = ORIENTED_EDGE ( 'NONE', *, *, #6654, .F. ) ;
#4897 = VERTEX_POINT ( 'NONE', #8536 ) ;
#4898 = MECHANICAL_DESIGN_GEOMETRIC_PRESENTATION_REPRESENTATION (  '', ( #10192 ), #9826 ) ;
#4899 = VECTOR ( 'NONE', #6065, 1000.000000000000000 ) ;
#4900 = LINE ( 'NONE', #4177, #6409 ) ;
#4901 = FACE_OUTER_BOUND ( 'NONE', #3999, .T. ) ;
#4902 = LINE ( 'NONE', #693, #771 ) ;
#4903 = EDGE_CURVE ( 'NONE', #7956, #8585, #420, .T. ) ;
#4904 = CARTESIAN_POINT ( 'NONE',  ( 25.00000000000000000, 1.000000000000000000, 0.000000000000000000 ) ) ;
#4905 = ADVANCED_FACE ( 'NONE', ( #9430, #4132 ), #8592, .T. ) ;
#4906 = LINE ( 'NONE', #5626, #2151 ) ;
#4907 = VECTOR ( 'NONE', #191, 1000.000000000000000 ) ;
#4908 = VERTEX_POINT ( 'NONE', #4633 ) ;
#4909 = ADVANCED_FACE ( 'NONE', ( #2938 ), #9061, .F. ) ;
#4910 = ORIENTED_EDGE ( 'NONE', *, *, #5514, .T. ) ;
#4911 = VECTOR ( 'NONE', #5061, 1000.000000000000114 ) ;
#4912 =( LENGTH_UNIT ( ) NAMED_UNIT ( * ) SI_UNIT ( .MILLI., .METRE. ) );
#4913 = LINE ( 'NONE', #3456, #5162 ) ;
#4914 = ORIENTED_EDGE ( 'NONE', *, *, #9276, .F. ) ;
#4915 = CARTESIAN_POINT ( 'NONE',  ( -0.5000000000000000000, 10.00000000000000355, -6.999999999999997335 ) ) ;
#4916 = SHAPE_DEFINITION_REPRESENTATION ( #6369, #7685 ) ;
#4917 = CARTESIAN_POINT ( 'NONE',  ( 25.00000000000000000, 2.612499998088169129, 0.000000000000000000 ) ) ;
#4918 = ORIENTED_EDGE ( 'NONE', *, *, #7546, .F. ) ;
#4919 = VECTOR ( 'NONE', #1069, 1000.000000000000000 ) ;
#4920 = DIRECTION ( 'NONE',  ( 0.000000000000000000, 0.000000000000000000, -1.000000000000000000 ) ) ;
#4921 = ADVANCED_FACE ( 'NONE', ( #10420 ), #207, .T. ) ;
#4922 = CARTESIAN_POINT ( 'NONE',  ( -17.40975659021752975, 1.593749999044084431, -17.40975659021752975 ) ) ;
#4923 = ORIENTED_EDGE ( 'NONE', *, *, #4156, .F. ) ;
#4924 = ORIENTED_EDGE ( 'NONE', *, *, #9689, .T. ) ;
#4925 = ORIENTED_EDGE ( 'NONE', *, *, #6294, .F. ) ;
#4926 = EDGE_CURVE ( 'NONE', #3614, #69, #8347, .T. ) ;
#4927 = CARTESIAN_POINT ( 'NONE',  ( 17.67766952966369232, 2.737499998088169573, -17.67766952966369232 ) ) ;
#4928 = DIRECTION ( 'NONE',  ( 1.000000000000000000, 0.000000000000000000, 0.000000000000000000 ) ) ;
#4929 = CARTESIAN_POINT ( 'NONE',  ( 17.40975659021752975, 3.343749999044085097, -17.40975659021752975 ) ) ;
#4930 = EDGE_LOOP ( 'NONE', ( #6773, #9877, #513, #8584 ) ) ;
#4931 = FACE_OUTER_BOUND ( 'NONE', #1738, .T. ) ;
#4932 =( NAMED_UNIT ( * ) SI_UNIT ( $, .STERADIAN. ) SOLID_ANGLE_UNIT ( ) );
#4933 = FACE_OUTER_BOUND ( 'NONE', #794, .T. ) ;
#4934 = ADVANCED_BREP_SHAPE_REPRESENTATION ( '', ( #10510, #7040 ), #4727 ) ;
#4935 = CARTESIAN_POINT ( 'NONE',  ( 87.32050807568876394, 92.28203230275514102, 0.000000000000000000 ) ) ;
#4936 = DIRECTION ( 'NONE',  ( 0.000000000000000000, 0.000000000000000000, 1.000000000000000000 ) ) ;
#4937 = DIRECTION ( 'NONE',  ( 0.000000000000000000, 0.000000000000000000, -1.000000000000000000 ) ) ;
#4938 = CARTESIAN_POINT ( 'NONE',  ( 0.000000000000000000, 10.00000000000000355, 0.000000000000000000 ) ) ;
#4939 = ORIENTED_EDGE ( 'NONE', *, *, #1471, .F. ) ;
#4940 = ORIENTED_EDGE ( 'NONE', *, *, #4163, .F. ) ;
#4941 = DIRECTION ( 'NONE',  ( 0.000000000000000000, 1.000000000000000000, 0.000000000000000000 ) ) ;
#4942 = PRODUCT_DEFINITION_CONTEXT ( 'detailed design', #8930, 'design' ) ;
#4943 = CARTESIAN_POINT ( 'NONE',  ( 10.19839929293506486, 3.206249999044084031, 24.62111388749999819 ) ) ;
#4944 = CARTESIAN_POINT ( 'NONE',  ( 0.000000000000000000, -1.026060429977008193, 0.000000000000000000 ) ) ;
#4945 = CARTESIAN_POINT ( 'NONE',  ( 0.000000000000000000, -8.528980942125404141, -24.91176187412963117 ) ) ;
#4946 = CIRCLE ( 'NONE', #3701, 2.999999999999999112 ) ;
#4947 = ADVANCED_FACE ( 'NONE', ( #2836 ), #1919, .F. ) ;
#4948 = AXIS2_PLACEMENT_3D ( 'NONE', #4881, #1500, #10784 ) ;
#4949 = EDGE_LOOP ( 'NONE', ( #10742, #3441, #2957 ) ) ;
#4950 = FACE_OUTER_BOUND ( 'NONE', #4696, .T. ) ;
#4951 = CARTESIAN_POINT ( 'NONE',  ( 6.386751345948063374, 10.00000000000000355, 11.06217782649112458 ) ) ;
#4952 = DIRECTION ( 'NONE',  ( 0.000000000000000000, 0.000000000000000000, 1.000000000000000000 ) ) ;
#4953 = PLANE ( 'NONE',  #8869 ) ;
#4954 = ORIENTED_EDGE ( 'NONE', *, *, #6588, .T. ) ;
#4955 = ORIENTED_EDGE ( 'NONE', *, *, #8893, .F. ) ;
#4956 = VECTOR ( 'NONE', #5370, 1000.000000000000000 ) ;
#4957 = AXIS2_PLACEMENT_3D ( 'NONE', #4767, #553, #3937 ) ;
#4958 = EDGE_LOOP ( 'NONE', ( #7001, #10808, #5594, #4530 ) ) ;
#4959 = CARTESIAN_POINT ( 'NONE',  ( 0.000000000000000000, 85.00000000000000000, 0.000000000000000000 ) ) ;
#4960 = CARTESIAN_POINT ( 'NONE',  ( -6.994037468151973691, 19.34316356887879351, 0.3335819196118008922 ) ) ;
#4961 = DIRECTION ( 'NONE',  ( 0.000000000000000000, 1.000000000000000000, -1.502202555303642096E-16 ) ) ;
#4962 = CIRCLE ( 'NONE', #1966, 2.999999999999998668 ) ;
#4963 = AXIS2_PLACEMENT_3D ( 'NONE', #10496, #5467, #4704 ) ;
#4964 = CARTESIAN_POINT ( 'NONE',  ( 1.530808498934191521E-15, 4.250000000000000000, -25.00000000000000000 ) ) ;
#4965 = DIRECTION ( 'NONE',  ( 0.000000000000000000, 0.000000000000000000, -1.000000000000000000 ) ) ;
#4966 = EDGE_LOOP ( 'NONE', ( #619, #7507 ) ) ;
#4967 = ORIENTED_EDGE ( 'NONE', *, *, #3148, .F. ) ;
#4968 = ADVANCED_FACE ( 'NONE', ( #2890 ), #7062, .T. ) ;
#4969 = EDGE_CURVE ( 'NONE', #10165, #2942, #6424, .T. ) ;
#4970 = VECTOR ( 'NONE', #6167, 1000.000000000000000 ) ;
#4971 = CARTESIAN_POINT ( 'NONE',  ( -15.74999999999997158, 25.00000000000000000, 3.000000000000162981 ) ) ;
#4972 = ORIENTED_EDGE ( 'NONE', *, *, #3989, .F. ) ;
#4973 = DIRECTION ( 'NONE',  ( -0.000000000000000000, 0.000000000000000000, -1.000000000000000000 ) ) ;
#4974 = DIRECTION ( 'NONE',  ( 0.000000000000000000, 0.000000000000000000, 1.000000000000000000 ) ) ;
#4975 = CARTESIAN_POINT ( 'NONE',  ( 11.16025403784440329, 90.66987298107783033, 5.000000000000000000 ) ) ;
#4976 = DIRECTION ( 'NONE',  ( -0.000000000000000000, -1.000000000000000000, -0.000000000000000000 ) ) ;
#4977 = CARTESIAN_POINT ( 'NONE',  ( -24.62111388750000174, 0.6562499990440845421, -10.19839929293506131 ) ) ;
#4978 = ADVANCED_FACE ( 'NONE', ( #1980 ), #6123, .F. ) ;
#4979 = ORIENTED_EDGE ( 'NONE', *, *, #2343, .F. ) ;
#4980 = AXIS2_PLACEMENT_3D ( 'NONE', #8005, #2951, #435 ) ;
#4981 = EDGE_LOOP ( 'NONE', ( #9024, #286, #2983, #8297 ) ) ;
#4982 = EDGE_CURVE ( 'NONE', #634, #7970, #6340, .T. ) ;
#4983 = CARTESIAN_POINT ( 'NONE',  ( -10.19839929293507552, 1.081249999044084475, 24.62111388749999463 ) ) ;
#4984 = CARTESIAN_POINT ( 'NONE',  ( 6.531088913245477023, 10.00000000000000355, 10.31217782649111214 ) ) ;
#4985 = CARTESIAN_POINT ( 'NONE',  ( 17.40975659021752975, 2.343749999044085097, -17.40975659021752975 ) ) ;
#4986 = DIRECTION ( 'NONE',  ( 0.000000000000000000, 1.000000000000000000, -0.000000000000000000 ) ) ;
#4987 = EDGE_LOOP ( 'NONE', ( #2565, #5464, #8523, #7870 ) ) ;
#4988 = LINE ( 'NONE', #6698, #4229 ) ;
#4989 = AXIS2_PLACEMENT_3D ( 'NONE', #1477, #7374, #2355 ) ;
#4990 = LINE ( 'NONE', #6589, #5966 ) ;
#4991 = DIRECTION ( 'NONE',  ( -0.000000000000000000, -1.000000000000000000, -0.000000000000000000 ) ) ;
#4992 = LINE ( 'NONE', #10785, #4272 ) ;
#4993 = DIRECTION ( 'NONE',  ( 0.8660254037844451469, 0.000000000000000000, 0.4999999999999887312 ) ) ;
#4994 = EDGE_CURVE ( 'NONE', #4112, #7330, #9224, .T. ) ;
#4995 = AXIS2_PLACEMENT_3D ( 'NONE', #753, #6723, #1744 ) ;
#4996 = AXIS2_PLACEMENT_3D ( 'NONE', #5909, #1056, #44 ) ;
#4997 = ORIENTED_EDGE ( 'NONE', *, *, #4473, .F. ) ;
#4998 = ORIENTED_EDGE ( 'NONE', *, *, #1016, .F. ) ;
#4999 = ORIENTED_EDGE ( 'NONE', *, *, #3833, .T. ) ;
#5000 = CIRCLE ( 'NONE', #2339, 0.1000000000000002554 ) ;
#5001 = ORIENTED_EDGE ( 'NONE', *, *, #9891, .T. ) ;
#5002 = CARTESIAN_POINT ( 'NONE',  ( -10.35533905932739174, 5.299999998088169129, 24.99999999999999289 ) ) ;
#5003 = AXIS2_PLACEMENT_3D ( 'NONE', #8916, #3044, #7209 ) ;
#5004 = CARTESIAN_POINT ( 'NONE',  ( 25.00000000000000000, 3.062500000000000000, -10.35533905932737753 ) ) ;
#5005 = CARTESIAN_POINT ( 'NONE',  ( -7.276923788646446845, 25.00000000000000000, 18.60400172474275848 ) ) ;
#5006 = CIRCLE ( 'NONE', #240, 24.91176187412963117 ) ;
#5007 = ADVANCED_FACE ( 'NONE', ( #4585 ), #6960, .T. ) ;
#5008 = CARTESIAN_POINT ( 'NONE',  ( -25.00000000000000000, 2.112499998088169129, -3.061616997868383043E-15 ) ) ;
#5009 = FACE_BOUND ( 'NONE', #10247, .T. ) ;
#5010 = CYLINDRICAL_SURFACE ( 'NONE', #384, 6.999999999999997335 ) ;
#5011 = AXIS2_PLACEMENT_3D ( 'NONE', #10100, #9153, #4364 ) ;
#5012 = CARTESIAN_POINT ( 'NONE',  ( 24.62111388750000174, 2.218749999044084653, 0.000000000000000000 ) ) ;
#5013 = CARTESIAN_POINT ( 'NONE',  ( 7.276923788646707969, 28.00000000000000000, 18.60400172474265190 ) ) ;
#5014 = ORIENTED_EDGE ( 'NONE', *, *, #9010, .F. ) ;
#5015 = ORIENTED_EDGE ( 'NONE', *, *, #6722, .F. ) ;
#5016 = AXIS2_PLACEMENT_3D ( 'NONE', #4348, #814, #2500 ) ;
#5017 = VERTEX_POINT ( 'NONE', #6237 ) ;
#5018 = ORIENTED_EDGE ( 'NONE', *, *, #3066, .T. ) ;
#5019 = CIRCLE ( 'NONE', #9606, 27.91176187412962761 ) ;
#5020 = CARTESIAN_POINT ( 'NONE',  ( -3.058047309050066165, 10.00000000000000355, 6.296693311223885203 ) ) ;
#5021 = SHAPE_REPRESENTATION ( 'Upper Stainless Steel Body Shell', ( #7040 ), #6327 ) ;
#5022 = AXIS2_PLACEMENT_3D ( 'NONE', #7933, #9542, #8809 ) ;
#5023 = CARTESIAN_POINT ( 'NONE',  ( 15.75000000000001421, 28.00000000000000000, 2.999999999999942268 ) ) ;
#5024 = CARTESIAN_POINT ( 'NONE',  ( 15.13990010960492505, 25.00000000000000000, 5.276923788646651126 ) ) ;
#5025 = CARTESIAN_POINT ( 'NONE',  ( 0.000000000000000000, 20.00000000000000355, 0.000000000000000000 ) ) ;
#5026 = LINE ( 'NONE', #757, #2672 ) ;
#5027 = ORIENTED_EDGE ( 'NONE', *, *, #3220, .T. ) ;
#5028 = FACE_OUTER_BOUND ( 'NONE', #6330, .T. ) ;
#5029 = CARTESIAN_POINT ( 'NONE',  ( -17.67766952966369232, 4.237499998088169129, 17.67766952966368876 ) ) ;
#5030 = CARTESIAN_POINT ( 'NONE',  ( -3.499999999999921396, 20.00000000000000355, -6.062177826491113919 ) ) ;
#5031 = ORIENTED_EDGE ( 'NONE', *, *, #8067, .F. ) ;
#5032 = CARTESIAN_POINT ( 'NONE',  ( 0.5000000000000000000, 19.03096903053430822, 6.982120021884467675 ) ) ;
#5033 = PRODUCT_CONTEXT ( 'NONE', #1587, 'mechanical' ) ;
#5034 = CARTESIAN_POINT ( 'NONE',  ( 17.10400172474269098, -0.001000000000001000089, 12.87499999999995381 ) ) ;
#5035 = CARTESIAN_POINT ( 'NONE',  ( 6.305607966083798921, 7.781088913245563177, 11.92163336986834743 ) ) ;
#5036 = CARTESIAN_POINT ( 'NONE',  ( 24.62111388750000174, 3.218749999044084653, 0.000000000000000000 ) ) ;
#5037 = EDGE_CURVE ( 'NONE', #3766, #3126, #8887, .T. ) ;
#5038 = EDGE_LOOP ( 'NONE', ( #9419, #10879, #3424, #875 ) ) ;
#5039 = EDGE_CURVE ( 'NONE', #1319, #9255, #8715, .T. ) ;
#5040 = DIRECTION ( 'NONE',  ( 1.000000000000000000, 0.000000000000000000, 0.000000000000000000 ) ) ;
#5041 = CARTESIAN_POINT ( 'NONE',  ( 17.40975659021752975, 0.3437499990440845421, -17.40975659021752975 ) ) ;
#5042 = DIRECTION ( 'NONE',  ( 0.4999999999999967248, 0.000000000000000000, -0.8660254037844404840 ) ) ;
#5043 = ORIENTED_EDGE ( 'NONE', *, *, #8094, .T. ) ;
#5044 = CARTESIAN_POINT ( 'NONE',  ( -3.223142256880076948E-15, 28.00000000000000000, -15.75000000000000000 ) ) ;
#5045 = SURFACE_STYLE_USAGE ( .BOTH. , #6752 ) ;
#5046 = CARTESIAN_POINT ( 'NONE',  ( -18.60400172474257730, 28.00000000000000000, 7.276923788646904256 ) ) ;
#5047 = CARTESIAN_POINT ( 'NONE',  ( 3.061616997868383043E-15, 8.000000000000003553, 25.00000000000000000 ) ) ;
#5048 = LINE ( 'NONE', #2324, #9378 ) ;
#5049 = DIRECTION ( 'NONE',  ( -0.5000000000000069944, 0.000000000000000000, 0.8660254037844344888 ) ) ;
#5050 = EDGE_CURVE ( 'NONE', #2606, #8513, #7836, .T. ) ;
#5051 = EDGE_CURVE ( 'NONE', #10543, #3961, #10831, .T. ) ;
#5052 = ADVANCED_FACE ( 'NONE', ( #5354 ), #5499, .F. ) ;
#5053 = ORIENTED_EDGE ( 'NONE', *, *, #8479, .F. ) ;
#5054 = VERTEX_POINT ( 'NONE', #1098 ) ;
#5055 = VERTEX_POINT ( 'NONE', #3623 ) ;
#5056 = EDGE_CURVE ( 'NONE', #2069, #6402, #2780, .T. ) ;
#5057 = CARTESIAN_POINT ( 'NONE',  ( 13.63990010960487353, 25.00000000000000000, -7.875000000000067502 ) ) ;
#5058 = CARTESIAN_POINT ( 'NONE',  ( 17.40975659021752975, 0.3437499990440845421, -17.40975659021752975 ) ) ;
#5059 = CARTESIAN_POINT ( 'NONE',  ( 10.19839929293506486, 2.206249999044084920, 24.62111388749999819 ) ) ;
#5060 = CARTESIAN_POINT ( 'NONE',  ( 24.62111388749999463, 1.156249999044084431, 10.19839929293507730 ) ) ;
#5061 = DIRECTION ( 'NONE',  ( -0.4330127018922172999, -0.8660254037844380415, -0.2500000000000054956 ) ) ;
#5062 = DIRECTION ( 'NONE',  ( 1.445602896647339163E-16, 0.000000000000000000, 1.000000000000000000 ) ) ;
#5063 = CYLINDRICAL_SURFACE ( 'NONE', #4082, 25.00000000000000000 ) ;
#5064 = CARTESIAN_POINT ( 'NONE',  ( 24.62111388750000174, 2.281249999044085541, -10.19839929293505776 ) ) ;
#5065 = EDGE_CURVE ( 'NONE', #859, #492, #9026, .T. ) ;
#5066 = DIRECTION ( 'NONE',  ( 0.000000000000000000, -0.8660254037844380415, -0.5000000000000009992 ) ) ;
#5067 = VERTEX_POINT ( 'NONE', #9797 ) ;
#5068 = VERTEX_POINT ( 'NONE', #3957 ) ;
#5069 = ORIENTED_EDGE ( 'NONE', *, *, #1129, .T. ) ;
#5070 = VERTEX_POINT ( 'NONE', #3045 ) ;
#5071 = ADVANCED_FACE ( 'NONE', ( #2228 ), #1654, .F. ) ;
#5072 = CARTESIAN_POINT ( 'NONE',  ( 0.000000000000000000, 7.000000000000003553, 0.000000000000000000 ) ) ;
#5073 = DIRECTION ( 'NONE',  ( 0.000000000000000000, 0.000000000000000000, 1.000000000000000000 ) ) ;
#5074 = CARTESIAN_POINT ( 'NONE',  ( 24.99999999999999289, 4.937500000000000888, 10.35533905932739529 ) ) ;
#5075 = ADVANCED_BREP_SHAPE_REPRESENTATION ( '', ( #3340, #7040 ), #8059 ) ;
#5076 = CARTESIAN_POINT ( 'NONE',  ( 24.81055694375000087, 0.5031249985661269131, 0.000000000000000000 ) ) ;
#5077 = CARTESIAN_POINT ( 'NONE',  ( 3.957930336368489021E-15, 25.00000000000000000, 19.75000000000000000 ) ) ;
#5078 = EDGE_LOOP ( 'NONE', ( #3127, #8413, #1178, #1705 ) ) ;
#5079 = SURFACE_STYLE_USAGE ( .BOTH. , #96 ) ;
#5080 = DIRECTION ( 'NONE',  ( 0.000000000000000000, -2.775557561562888270E-17, -1.000000000000000000 ) ) ;
#5081 = DIRECTION ( 'NONE',  ( 0.8660254037844399289, -0.000000000000000000, 0.4999999999999977796 ) ) ;
#5082 = ORIENTED_EDGE ( 'NONE', *, *, #1623, .F. ) ;
#5083 = FACE_OUTER_BOUND ( 'NONE', #1770, .T. ) ;
#5084 = CARTESIAN_POINT ( 'NONE',  ( 0.000000000000000000, 28.00000000000000000, -5.999999999999999112 ) ) ;
#5085 = DIRECTION ( 'NONE',  ( 0.000000000000000000, 0.000000000000000000, 1.000000000000000000 ) ) ;
#5086 = CARTESIAN_POINT ( 'NONE',  ( 82.32050807568876394, 89.28203230275514102, 5.000000000000000000 ) ) ;
#5087 = VERTEX_POINT ( 'NONE', #1353 ) ;
#5088 = VECTOR ( 'NONE', #9126, 1000.000000000000000 ) ;
#5089 = CARTESIAN_POINT ( 'NONE',  ( -15.60400172474251868, 25.00000000000000000, 12.47307621135349720 ) ) ;
#5090 = CARTESIAN_POINT ( 'NONE',  ( -4.592425496802574367E-15, 1.362499998088169129, 25.00000000000000000 ) ) ;
#5091 = PLANE ( 'NONE',  #2177 ) ;
#5092 = ORIENTED_EDGE ( 'NONE', *, *, #7757, .T. ) ;
#5093 = CARTESIAN_POINT ( 'NONE',  ( -4.592425496802574367E-15, 3.750000000000000000, 25.00000000000000000 ) ) ;
#5094 =( NAMED_UNIT ( * ) SI_UNIT ( $, .STERADIAN. ) SOLID_ANGLE_UNIT ( ) );
#5095 = CARTESIAN_POINT ( 'NONE',  ( -0.5590169943749458970, 0.000000000000000000, 0.000000000000000000 ) ) ;
#5096 = CARTESIAN_POINT ( 'NONE',  ( 17.67766952966369232, 1.737499998088169351, -17.67766952966369232 ) ) ;
#5097 = DIRECTION ( 'NONE',  ( 1.000000000000000000, 0.000000000000000000, 0.000000000000000000 ) ) ;
#5098 = CARTESIAN_POINT ( 'NONE',  ( 87.32050807568876394, 89.28203230275514102, 0.000000000000000000 ) ) ;
#5099 = ORIENTED_EDGE ( 'NONE', *, *, #797, .F. ) ;
#5100 = ORIENTED_EDGE ( 'NONE', *, *, #3392, .T. ) ;
#5101 = VERTEX_POINT ( 'NONE', #626 ) ;
#5102 = CYLINDRICAL_SURFACE ( 'NONE', #1221, 5.000000000000005329 ) ;
#5103 = CARTESIAN_POINT ( 'NONE',  ( 1.507608415688466075E-15, 3.643749999044084920, -24.62111388750000174 ) ) ;
#5104 = DIRECTION ( 'NONE',  ( 0.000000000000000000, 0.000000000000000000, 1.000000000000000000 ) ) ;
#5105 = ADVANCED_FACE ( 'NONE', ( #2992 ), #4690, .F. ) ;
#5106 = CARTESIAN_POINT ( 'NONE',  ( -24.62111388750000174, 0.8937499990440845865, -3.015216831376932151E-15 ) ) ;
#5107 = CARTESIAN_POINT ( 'NONE',  ( 17.67766952966368521, 0.8750000000000000000, 17.67766952966369232 ) ) ;
#5108 = ORIENTED_EDGE ( 'NONE', *, *, #5539, .T. ) ;
#5109 = CARTESIAN_POINT ( 'NONE',  ( -17.67766952966369232, 2.237499998088169573, 17.67766952966368876 ) ) ;
#5110 = CARTESIAN_POINT ( 'NONE',  ( 0.000000000000000000, 20.00000000000000355, 0.000000000000000000 ) ) ;
#5111 = CARTESIAN_POINT ( 'NONE',  ( 24.99999999999999289, 0.9374999999999998890, 10.35533905932739529 ) ) ;
#5112 = DIRECTION ( 'NONE',  ( 0.7071067811865470176, 0.3535533905932748411, -0.6123724356957946924 ) ) ;
#5113 = AXIS2_PLACEMENT_3D ( 'NONE', #9783, #6529, #10285 ) ;
#5114 = EDGE_CURVE ( 'NONE', #6661, #5087, #9078, .T. ) ;
#5115 = VERTEX_POINT ( 'NONE', #2285 ) ;
#5116 = ORIENTED_EDGE ( 'NONE', *, *, #8153, .T. ) ;
#5117 = ORIENTED_EDGE ( 'NONE', *, *, #8221, .F. ) ;
#5118 = CARTESIAN_POINT ( 'NONE',  ( 2.694222958124177204E-15, 5.000000000000000000, 22.00000000000000355 ) ) ;
#5119 = VECTOR ( 'NONE', #2863, 1000.000000000000114 ) ;
#5120 = CIRCLE ( 'NONE', #4429, 6.999999999999997335 ) ;
#5121 = EDGE_CURVE ( 'NONE', #399, #3717, #775, .T. ) ;
#5122 = DIRECTION ( 'NONE',  ( -0.000000000000000000, 1.000000000000000000, -0.000000000000000000 ) ) ;
#5123 = ORIENTED_EDGE ( 'NONE', *, *, #9421, .T. ) ;
#5124 = CARTESIAN_POINT ( 'NONE',  ( 3.208128317448888378, 19.34316356887880772, 6.223805082245760012 ) ) ;
#5125 = CARTESIAN_POINT ( 'NONE',  ( 12.47307621135322186, 25.00000000000000000, -15.60400172474273717 ) ) ;
#5126 = ADVANCED_FACE ( 'NONE', ( #1401 ), #3215, .T. ) ;
#5127 = CARTESIAN_POINT ( 'NONE',  ( 5.510910596163089556E-16, 10.10000000000000497, 4.500000000000000888 ) ) ;
#5128 = DIRECTION ( 'NONE',  ( 0.9819805060619676285, 0.000000000000000000, -0.1889822365046036623 ) ) ;
#5129 = PLANE ( 'NONE',  #9198 ) ;
#5130 = EDGE_CURVE ( 'NONE', #2588, #5479, #8355, .T. ) ;
#5131 = CIRCLE ( 'NONE', #2978, 5.000000000000000000 ) ;
#5132 = AXIS2_PLACEMENT_3D ( 'NONE', #7618, #1061, #2525 ) ;
#5133 = ORIENTED_EDGE ( 'NONE', *, *, #3561, .T. ) ;
#5134 = EDGE_LOOP ( 'NONE', ( #4162, #8367, #10754, #3993 ) ) ;
#5135 = AXIS2_PLACEMENT_3D ( 'NONE', #3448, #3627, #266 ) ;
#5136 = PLANE ( 'NONE',  #6727 ) ;
#5137 = CARTESIAN_POINT ( 'NONE',  ( -25.00000000000000000, 4.437500000000001776, -10.35533905932738108 ) ) ;
#5138 = CIRCLE ( 'NONE', #696, 28.00000000000000000 ) ;
#5139 = DIRECTION ( 'NONE',  ( 0.000000000000000000, 0.000000000000000000, 1.000000000000000000 ) ) ;
#5140 = DIRECTION ( 'NONE',  ( 0.000000000000000000, -1.000000000000000000, 0.000000000000000000 ) ) ;
#5141 = PRODUCT_CONTEXT ( 'NONE', #3263, 'mechanical' ) ;
#5142 = DIRECTION ( 'NONE',  ( 0.000000000000000000, -0.000000000000000000, -1.000000000000000000 ) ) ;
#5143 = EDGE_LOOP ( 'NONE', ( #2724, #10053, #1091, #3698 ) ) ;
#5144 = EDGE_CURVE ( 'NONE', #5055, #8118, #1311, .T. ) ;
#5145 = FACE_BOUND ( 'NONE', #5278, .T. ) ;
#5146 = DIRECTION ( 'NONE',  ( 0.000000000000000000, 1.000000000000000000, -0.000000000000000000 ) ) ;
#5147 = VECTOR ( 'NONE', #4879, 1000.000000000000114 ) ;
#5148 =( BOUNDED_CURVE ( )  B_SPLINE_CURVE ( 2, ( #1363, #3270, #642, #7431, #6615, #1573, #10814, #4860, #4964 ),
 .UNSPECIFIED., .F., .F. ) 
 B_SPLINE_CURVE_WITH_KNOTS ( ( 3, 2, 2, 2, 3 ),
 ( 0.7500000000000000000, 0.7750000000000000222, 0.8000000000000000444, 0.8250000000000000666, 0.8500000000000000888 ),
 .UNSPECIFIED. ) 
 CURVE ( )  GEOMETRIC_REPRESENTATION_ITEM ( )  RATIONAL_B_SPLINE_CURVE ( ( 1.000000000000000000, 0.9238795325112867385, 1.000000000000000000, 0.9238795325112867385, 1.000000000000000000, 0.9238795325112867385, 1.000000000000000000, 0.9238795325112864054, 1.000000000000000444 ) ) 
 REPRESENTATION_ITEM ( '' )  );
#5149 = CARTESIAN_POINT ( 'NONE',  ( 24.62111388750000174, 1.456249999044084475, -10.19839929293505776 ) ) ;
#5150 = DIRECTION ( 'NONE',  ( 0.000000000000000000, -0.000000000000000000, 1.000000000000000000 ) ) ;
#5151 = CARTESIAN_POINT ( 'NONE',  ( 10.35533905932738286, 2.812500000000000000, 24.99999999999999645 ) ) ;
#5152 = CARTESIAN_POINT ( 'NONE',  ( 0.000000000000000000, 85.00000000000000000, -30.00000000000000000 ) ) ;
#5153 = ORIENTED_EDGE ( 'NONE', *, *, #10095, .F. ) ;
#5154 = CARTESIAN_POINT ( 'NONE',  ( -4.592425496802574367E-15, 1.362499998088169129, 25.00000000000000000 ) ) ;
#5155 = FILL_AREA_STYLE ('',( #8562 ) ) ;
#5156 = CARTESIAN_POINT ( 'NONE',  ( 1.399999999999998579, -2.081668171172168513E-16, -7.500000000000007994 ) ) ;
#5157 = CARTESIAN_POINT ( 'NONE',  ( 1.530808498934191521E-15, 1.862499998088169129, -25.00000000000000000 ) ) ;
#5158 = LINE ( 'NONE', #9399, #6743 ) ;
#5159 = CARTESIAN_POINT ( 'NONE',  ( -4.592425496802574367E-15, 3.750000000000000000, 25.00000000000000000 ) ) ;
#5160 = CIRCLE ( 'NONE', #9728, 24.91176187412963117 ) ;
#5161 = ORIENTED_EDGE ( 'NONE', *, *, #1135, .F. ) ;
#5163 = ORIENTED_EDGE ( 'NONE', *, *, #10771, .F. ) ;
#5162 = VECTOR ( 'NONE', #5081, 1000.000000000000114 ) ;
#5164 = VERTEX_POINT ( 'NONE', #573 ) ;
#5165 = ORIENTED_EDGE ( 'NONE', *, *, #3849, .T. ) ;
#5166 = CARTESIAN_POINT ( 'NONE',  ( 0.000000000000000000, 85.00000000000000000, 0.000000000000000000 ) ) ;
#5167 = CARTESIAN_POINT ( 'NONE',  ( -24.62111388750000174, 2.831249999044084475, -10.19839929293506131 ) ) ;
#5168 = CIRCLE ( 'NONE', #3919, 25.00000000000000000 ) ;
#5169 = CARTESIAN_POINT ( 'NONE',  ( 24.62111388750000174, 0.4562499990440845865, -10.19839929293505776 ) ) ;
#5170 = CARTESIAN_POINT ( 'NONE',  ( -10.19839929293505776, 2.706249999044084475, -24.62111388750000174 ) ) ;
#5171 = CARTESIAN_POINT ( 'NONE',  ( 10.35533905932737930, 1.187500000000000444, -25.00000000000000000 ) ) ;
#5172 = FILL_AREA_STYLE ('',( #6823 ) ) ;
#5173 = DIRECTION ( 'NONE',  ( -0.000000000000000000, 1.000000000000000000, -0.000000000000000000 ) ) ;
#5174 = CIRCLE ( 'NONE', #3933, 7.500000000000000888 ) ;
#5175 = DIRECTION ( 'NONE',  ( 0.000000000000000000, 0.000000000000000000, -1.000000000000000000 ) ) ;
#5176 = FACE_OUTER_BOUND ( 'NONE', #6926, .T. ) ;
#5177 = CARTESIAN_POINT ( 'NONE',  ( -17.40975659021752975, 4.593749999044084653, -17.40975659021752975 ) ) ;
#5178 = CARTESIAN_POINT ( 'NONE',  ( -25.00000000000000000, 3.049999998088169129, -10.35533905932738108 ) ) ;
#5179 = CIRCLE ( 'NONE', #3751, 7.400000000000007461 ) ;
#5180 = ORIENTED_EDGE ( 'NONE', *, *, #3616, .F. ) ;
#5181 = CIRCLE ( 'NONE', #3752, 25.00000000000000000 ) ;
#5182 = ORIENTED_EDGE ( 'NONE', *, *, #9280, .T. ) ;
#5183 = EDGE_CURVE ( 'NONE', #631, #4407, #4486, .T. ) ;
#5184 = VERTEX_POINT ( 'NONE', #521 ) ;
#5185 = ORIENTED_EDGE ( 'NONE', *, *, #7857, .T. ) ;
#5186 = CIRCLE ( 'NONE', #9920, 5.349378127920655146 ) ;
#5187 = DIRECTION ( 'NONE',  ( 0.000000000000000000, -2.775557561562887961E-17, -1.000000000000000000 ) ) ;
#5188 = CIRCLE ( 'NONE', #42, 0.7499999999999997780 ) ;
#5189 = EDGE_CURVE ( 'NONE', #10065, #9967, #7211, .T. ) ;
#5190 = AXIS2_PLACEMENT_3D ( 'NONE', #1565, #3207, #6778 ) ;
#5191 = DIRECTION ( 'NONE',  ( -1.000000000000000000, 0.000000000000000000, -0.000000000000000000 ) ) ;
#5192 = VERTEX_POINT ( 'NONE', #3204 ) ;
#5193 = CYLINDRICAL_SURFACE ( 'NONE', #7650, 4.999999999999997335 ) ;
#5194 = DIRECTION ( 'NONE',  ( 0.000000000000000000, 0.000000000000000000, 1.000000000000000000 ) ) ;
#5195 = CARTESIAN_POINT ( 'NONE',  ( 0.000000000000000000, 25.00000000000000355, 0.000000000000000000 ) ) ;
#5196 = CARTESIAN_POINT ( 'NONE',  ( 7.347880794884118750E-16, 25.00000000000000000, 5.999999999999999112 ) ) ;
#5197 = CARTESIAN_POINT ( 'NONE',  ( 20.15540488255180307, 5.000000000000000000, 14.56419990634798900 ) ) ;
#5198 = VECTOR ( 'NONE', #694, 1000.000000000000000 ) ;
#5199 = ADVANCED_FACE ( 'NONE', ( #10737 ), #3899, .T. ) ;
#5200 = EDGE_CURVE ( 'NONE', #7304, #2289, #3150, .T. ) ;
#5201 = AXIS2_PLACEMENT_3D ( 'NONE', #5475, #8839, #1281 ) ;
#5202 = ORIENTED_EDGE ( 'NONE', *, *, #9998, .T. ) ;
#5203 = AXIS2_PLACEMENT_3D ( 'NONE', #5622, #7428, #7317 ) ;
#5204 = EDGE_CURVE ( 'NONE', #2942, #8620, #5188, .T. ) ;
#5205 = CARTESIAN_POINT ( 'NONE',  ( 1.500000000000001332, 0.000000000000000000, 0.000000000000000000 ) ) ;
#5206 = DIRECTION ( 'NONE',  ( -0.000000000000000000, -1.000000000000000000, -0.000000000000000000 ) ) ;
#5207 = CARTESIAN_POINT ( 'NONE',  ( -10.19839929293507375, 2.081249999044084920, 24.62111388749999108 ) ) ;
#5208 = CARTESIAN_POINT ( 'NONE',  ( -5.000000000000000000, 0.000000000000000000, -5.000000000000000000 ) ) ;
#5209 = LINE ( 'NONE', #5034, #1305 ) ;
#5210 = CARTESIAN_POINT ( 'NONE',  ( -17.67766952966368876, 4.987499998088170017, -17.67766952966369232 ) ) ;
#5211 = EDGE_CURVE ( 'NONE', #5055, #9481, #6392, .T. ) ;
#5212 =( REPRESENTATION_RELATIONSHIP ('NONE','NONE', #1269, #5021 ) REPRESENTATION_RELATIONSHIP_WITH_TRANSFORMATION ( #942 )SHAPE_REPRESENTATION_RELATIONSHIP( ) );
#5213 = CARTESIAN_POINT ( 'NONE',  ( -24.62111388750000884, 3.956249999044084920, 10.19839929293505421 ) ) ;
#5214 = CARTESIAN_POINT ( 'NONE',  ( 0.000000000000000000, 28.00000000000000000, -5.999999999999999112 ) ) ;
#5215 = CARTESIAN_POINT ( 'NONE',  ( 24.99999999999999289, 2.937500000000000000, 10.35533905932739529 ) ) ;
#5216 = CARTESIAN_POINT ( 'NONE',  ( -1.500000000000001332, 0.000000000000000000, 0.000000000000000000 ) ) ;
#5217 = EDGE_LOOP ( 'NONE', ( #1092, #291, #10693, #5926, #603, #3195, #3236, #7908, #10400 ) ) ;
#5218 = CARTESIAN_POINT ( 'NONE',  ( -25.00000000000000000, 3.500000000000000000, -3.061616997868383043E-15 ) ) ;
#5219 = PRESENTATION_STYLE_ASSIGNMENT (( #4441 ) ) ;
#5220 = CARTESIAN_POINT ( 'NONE',  ( 67.32050807568876394, 92.28203230275514102, 5.000000000000000000 ) ) ;
#5221 = CARTESIAN_POINT ( 'NONE',  ( 24.62111388750000174, 0.2812499990440845421, -10.19839929293505776 ) ) ;
#5222 = DIRECTION ( 'NONE',  ( -0.9659258262890684232, 0.2588190451025202399, 0.000000000000000000 ) ) ;
#5223 = CYLINDRICAL_SURFACE ( 'NONE', #1809, 2.999999999999997335 ) ;
#5224 = CARTESIAN_POINT ( 'NONE',  ( 17.67766952966368521, 3.875000000000000000, 17.67766952966369232 ) ) ;
#5225 =( BOUNDED_CURVE ( )  B_SPLINE_CURVE ( 2, ( #9222, #3533, #6699, #6928, #10286, #10055, #2968, #2702, #6099 ),
 .UNSPECIFIED., .F., .F. ) 
 B_SPLINE_CURVE_WITH_KNOTS ( ( 3, 2, 2, 2, 3 ),
 ( 0.1499999999999999944, 0.1749999999999999889, 0.2000000000000000111, 0.2249999999999999778, 0.2499999999999999722 ),
 .UNSPECIFIED. ) 
 CURVE ( )  GEOMETRIC_REPRESENTATION_ITEM ( )  RATIONAL_B_SPLINE_CURVE ( ( 1.000000000000000000, 0.9238795325112867385, 1.000000000000000000, 0.9238795325112867385, 1.000000000000000000, 0.9238795325112867385, 1.000000000000000000, 0.9238795325112868495, 0.9999999999999998890 ) ) 
 REPRESENTATION_ITEM ( '' )  );
#5226 = VERTEX_POINT ( 'NONE', #3096 ) ;
#5227 = EDGE_CURVE ( 'NONE', #7707, #7572, #9205, .T. ) ;
#5228 = CYLINDRICAL_SURFACE ( 'NONE', #6338, 7.500000000000000888 ) ;
#5229 = CARTESIAN_POINT ( 'NONE',  ( -10.19839929293507552, 4.081249999044084475, 24.62111388749999463 ) ) ;
#5230 = CARTESIAN_POINT ( 'NONE',  ( -2.999999999999999112, 25.00000000000000000, -19.75000000000000000 ) ) ;
#5231 = CARTESIAN_POINT ( 'NONE',  ( 25.00000000000000000, 4.612499998088169129, 0.000000000000000000 ) ) ;
#5232 = CARTESIAN_POINT ( 'NONE',  ( 24.62111388749999463, 5.156249999044083765, 10.19839929293507730 ) ) ;
#5233 = DIRECTION ( 'NONE',  ( 0.000000000000000000, 0.000000000000000000, 1.000000000000000000 ) ) ;
#5234 = DIRECTION ( 'NONE',  ( -0.8838834764831809965, 0.3535533905932741749, -0.3061862178479068386 ) ) ;
#5235 = CARTESIAN_POINT ( 'NONE',  ( -0.5000000000000000000, 10.00000000000000355, -12.19615242270663735 ) ) ;
#5236 = CARTESIAN_POINT ( 'NONE',  ( -20.63749999999999574, 0.000000000000000000, 0.000000000000000000 ) ) ;
#5237 = DIRECTION ( 'NONE',  ( 0.000000000000000000, 0.000000000000000000, 1.000000000000000000 ) ) ;
#5238 = CARTESIAN_POINT ( 'NONE',  ( 10.35533905932738286, 0.8125000000000001110, 24.99999999999999645 ) ) ;
#5239 = LINE ( 'NONE', #4528, #9210 ) ;
#5240 = VERTEX_POINT ( 'NONE', #9960 ) ;
#5241 = EDGE_LOOP ( 'NONE', ( #3363, #8183, #9243, #8626 ) ) ;
#5242 = VERTEX_POINT ( 'NONE', #7744 ) ;
#5243 = CARTESIAN_POINT ( 'NONE',  ( 15.60400172474269453, 25.00000000000000000, 12.47307621135327693 ) ) ;
#5244 = CARTESIAN_POINT ( 'NONE',  ( 19.75000000000000000, 28.00000000000000000, -7.291468677852036884E-14 ) ) ;
#5245 = ORIENTED_EDGE ( 'NONE', *, *, #6186, .F. ) ;
#5246 = DIRECTION ( 'NONE',  ( 0.000000000000000000, -1.000000000000000000, 0.000000000000000000 ) ) ;
#5247 = LINE ( 'NONE', #3567, #4844 ) ;
#5248 = CARTESIAN_POINT ( 'NONE',  ( 2.500000000000000444, 1.000000000000002220, -0.5773502691896270633 ) ) ;
#5249 = PLANE ( 'NONE',  #6017 ) ;
#5250 = PLANE ( 'NONE',  #3568 ) ;
#5251 = EDGE_CURVE ( 'NONE', #7391, #2965, #3597, .T. ) ;
#5252 = CARTESIAN_POINT ( 'NONE',  ( -10.19839929293507552, 5.081249999044084475, 24.62111388749999463 ) ) ;
#5253 = EDGE_LOOP ( 'NONE', ( #2522, #8627, #10665, #1 ) ) ;
#5254 = DIRECTION ( 'NONE',  ( -1.000000000000000000, -0.000000000000000000, -7.228014483236695816E-17 ) ) ;
#5255 = CARTESIAN_POINT ( 'NONE',  ( -10.19839929293505776, 1.706249999044084698, -24.62111388750000174 ) ) ;
#5256 = ORIENTED_EDGE ( 'NONE', *, *, #5786, .F. ) ;
#5257 = EDGE_CURVE ( 'NONE', #9174, #5713, #10014, .T. ) ;
#5258 = CARTESIAN_POINT ( 'NONE',  ( -6.296693311223874545, 19.03096903053432598, -3.058047309050087925 ) ) ;
#5259 = EDGE_CURVE ( 'NONE', #8587, #4079, #9183, .T. ) ;
#5260 = DIRECTION ( 'NONE',  ( 0.000000000000000000, 1.000000000000000000, 0.000000000000000000 ) ) ;
#5261 = DIRECTION ( 'NONE',  ( -0.5000000000000069944, 0.000000000000000000, 0.8660254037844344888 ) ) ;
#5262 = EDGE_CURVE ( 'NONE', #9883, #7721, #943, .T. ) ;
#5263 = CARTESIAN_POINT ( 'NONE',  ( -10.00000000000000000, 93.00000000000001421, 0.000000000000000000 ) ) ;
#5264 = VECTOR ( 'NONE', #9926, 1000.000000000000000 ) ;
#5265 = CARTESIAN_POINT ( 'NONE',  ( 17.40975659021752620, 5.093749999044084653, 17.40975659021753330 ) ) ;
#5266 = CARTESIAN_POINT ( 'NONE',  ( -10.19839929293507375, 1.081249999044084475, 24.62111388749999108 ) ) ;
#5267 = ORIENTED_EDGE ( 'NONE', *, *, #1016, .T. ) ;
#5268 = ADVANCED_FACE ( 'NONE', ( #3653 ), #1950, .F. ) ;
#5269 = CARTESIAN_POINT ( 'NONE',  ( -25.00000000000000000, 3.437500000000000000, -10.35533905932738108 ) ) ;
#5270 = DIRECTION ( 'NONE',  ( 0.000000000000000000, -1.000000000000000000, 0.000000000000000000 ) ) ;
#5271 = VECTOR ( 'NONE', #10476, 999.9999999999998863 ) ;
#5272 = CARTESIAN_POINT ( 'NONE',  ( 0.000000000000000000, 28.00000000000000000, 0.000000000000000000 ) ) ;
#5273 = DIRECTION ( 'NONE',  ( 0.000000000000000000, 0.000000000000000000, 1.000000000000000000 ) ) ;
#5274 = CARTESIAN_POINT ( 'NONE',  ( 24.99999999999999289, 2.937500000000000444, 10.35533905932739529 ) ) ;
#5275 = EDGE_CURVE ( 'NONE', #10413, #1987, #1621, .T. ) ;
#5276 = ORIENTED_EDGE ( 'NONE', *, *, #1732, .F. ) ;
#5277 = ORIENTED_EDGE ( 'NONE', *, *, #8492, .F. ) ;
#5278 = EDGE_LOOP ( 'NONE', ( #2752, #3631 ) ) ;
#5279 = AXIS2_PLACEMENT_3D ( 'NONE', #7793, #7611, #828 ) ;
#5280 = DIRECTION ( 'NONE',  ( 0.000000000000000000, 1.000000000000000000, 0.000000000000000000 ) ) ;
#5281 = CARTESIAN_POINT ( 'NONE',  ( -4.522825247065398226E-15, 4.143749999044084475, 24.62111388750000174 ) ) ;
#5282 = CARTESIAN_POINT ( 'NONE',  ( 0.000000000000000000, 0.000000000000000000, -25.00000000000000000 ) ) ;
#5283 = CARTESIAN_POINT ( 'NONE',  ( 17.67766952966369232, 3.737499998088169573, -17.67766952966369232 ) ) ;
#5284 = CARTESIAN_POINT ( 'NONE',  ( 17.40975659021752975, 4.343749999044084653, -17.40975659021752975 ) ) ;
#5285 = CARTESIAN_POINT ( 'NONE',  ( 0.000000000000000000, 82.00000000000000000, 0.000000000000000000 ) ) ;
#5286 = VERTEX_POINT ( 'NONE', #10344 ) ;
#5287 = LINE ( 'NONE', #4460, #8611 ) ;
#5288 = DIRECTION ( 'NONE',  ( -0.000000000000000000, 1.000000000000000000, -0.000000000000000000 ) ) ;
#5289 = CARTESIAN_POINT ( 'NONE',  ( 6.296693311223917178, 10.00000000000000355, -3.058047309049999996 ) ) ;
#5290 = CARTESIAN_POINT ( 'NONE',  ( 0.000000000000000000, 7.000000000000003553, 12.77350269189627063 ) ) ;
#5291 = VECTOR ( 'NONE', #6045, 1000.000000000000000 ) ;
#5292 = CARTESIAN_POINT ( 'NONE',  ( 24.62111388750000174, 4.281249999044084653, -10.19839929293505776 ) ) ;
#5293 = FACE_OUTER_BOUND ( 'NONE', #2080, .T. ) ;
#5294 = ORIENTED_EDGE ( 'NONE', *, *, #8221, .T. ) ;
#5295 = VERTEX_POINT ( 'NONE', #2438 ) ;
#5296 = CARTESIAN_POINT ( 'NONE',  ( -3.355508642977535150, 19.66631150450993104, 6.145599950363565434 ) ) ;
#5297 = CARTESIAN_POINT ( 'NONE',  ( 0.000000000000000000, 5.000000000000000000, 0.000000000000000000 ) ) ;
#5298 = EDGE_LOOP ( 'NONE', ( #10761, #10694, #1346, #2654 ) ) ;
#5299 = DIRECTION ( 'NONE',  ( 1.000000000000000000, 0.000000000000000000, 0.000000000000000000 ) ) ;
#5300 = DIRECTION ( 'NONE',  ( -0.000000000000000000, -1.000000000000000000, -0.000000000000000000 ) ) ;
#5301 = DIRECTION ( 'NONE',  ( 0.000000000000000000, -1.000000000000000000, 0.000000000000000000 ) ) ;
#5302 = ADVANCED_FACE ( 'NONE', ( #4443, #6864, #741, #7865, #10288, #9517, #6653, #8564, #5009, #1012, #2703, #802, #10222, #3255 ), #2640, .T. ) ;
#5303 = DIRECTION ( 'NONE',  ( -0.8660254037844327124, 0.000000000000000000, 0.5000000000000103251 ) ) ;
#5304 = DIRECTION ( 'NONE',  ( 0.000000000000000000, 0.000000000000000000, 1.000000000000000000 ) ) ;
#5305 = CARTESIAN_POINT ( 'NONE',  ( 10.19839929293506486, 4.206249999044084475, 24.62111388749999819 ) ) ;
#5306 = ORIENTED_EDGE ( 'NONE', *, *, #2274, .F. ) ;
#5307 = ORIENTED_EDGE ( 'NONE', *, *, #4385, .F. ) ;
#5308 = VERTEX_POINT ( 'NONE', #6036 ) ;
#5309 = DIRECTION ( 'NONE',  ( 0.000000000000000000, -2.775557561562888270E-17, -1.000000000000000000 ) ) ;
#5310 = CARTESIAN_POINT ( 'NONE',  ( -24.62111388750000884, 2.956249999044084475, 10.19839929293505421 ) ) ;
#5311 = CARTESIAN_POINT ( 'NONE',  ( 9.633606397919612263, 10.00000000000000355, 2.262820851736541350 ) ) ;
#5312 = CARTESIAN_POINT ( 'NONE',  ( 82.32050807568876394, 92.28203230275514102, 0.000000000000000000 ) ) ;
#5313 = CIRCLE ( 'NONE', #2351, 2.999999999999999112 ) ;
#5314 = AXIS2_PLACEMENT_3D ( 'NONE', #10677, #2063, #3035 ) ;
#5315 = DIRECTION ( 'NONE',  ( 0.8660254037844327124, 0.000000000000000000, -0.5000000000000103251 ) ) ;
#5316 = CARTESIAN_POINT ( 'NONE',  ( 17.10400172474269098, 28.00000000000000000, 12.87499999999995559 ) ) ;
#5317 = ADVANCED_FACE ( 'NONE', ( #6100 ), #4511, .F. ) ;
#5318 = AXIS2_PLACEMENT_3D ( 'NONE', #6217, #2918, #2969 ) ;
#5319 = AXIS2_PLACEMENT_3D ( 'NONE', #1870, #988, #7067 ) ;
#5320 = CARTESIAN_POINT ( 'NONE',  ( 19.74999999999998934, 28.00000000000000000, -3.000000000000067946 ) ) ;
#5321 = CARTESIAN_POINT ( 'NONE',  ( 24.62111388749999463, 5.156249999044083765, 10.19839929293507730 ) ) ;
#5322 = CARTESIAN_POINT ( 'NONE',  ( 10.19839929293505953, 0.5812499990440844755, -24.62111388750000174 ) ) ;
#5323 = VERTEX_POINT ( 'NONE', #4381 ) ;
#5324 = DIRECTION ( 'NONE',  ( 0.8660254037844327124, 0.000000000000000000, -0.5000000000000103251 ) ) ;
#5325 = EDGE_CURVE ( 'NONE', #10743, #2663, #4448, .T. ) ;
#5326 = CARTESIAN_POINT ( 'NONE',  ( -25.00000000000000000, 2.500000000000000000, -3.061616997868383043E-15 ) ) ;
#5327 = DIRECTION ( 'NONE',  ( -1.000000000000000000, 0.000000000000000000, 1.069128445102650095E-14 ) ) ;
#5328 = CARTESIAN_POINT ( 'NONE',  ( -17.67766952966369232, 1.237499998088169129, 17.67766952966368876 ) ) ;
#5329 = CIRCLE ( 'NONE', #8663, 12.77350269189627063 ) ;
#5330 = CIRCLE ( 'NONE', #3905, 15.00000000000000178 ) ;
#5331 = ORIENTED_EDGE ( 'NONE', *, *, #10318, .F. ) ;
#5332 = ORIENTED_EDGE ( 'NONE', *, *, #6602, .T. ) ;
#5333 = EDGE_CURVE ( 'NONE', #3965, #1976, #2366, .T. ) ;
#5334 = CARTESIAN_POINT ( 'NONE',  ( -17.40975659021753330, 1.843749999044084653, 17.40975659021752975 ) ) ;
#5335 = DIRECTION ( 'NONE',  ( 0.6546536707079774198, -0.000000000000000000, 0.7559289460184541731 ) ) ;
#5336 = CARTESIAN_POINT ( 'NONE',  ( -25.00000000000000000, 3.112499998088169129, -3.061616997868383043E-15 ) ) ;
#5337 = CARTESIAN_POINT ( 'NONE',  ( 17.67766952966369232, 0.1249999999999999722, -17.67766952966369232 ) ) ;
#5338 = CARTESIAN_POINT ( 'NONE',  ( -2.999999999999999112, -0.001000000000001000089, -19.75000000000000000 ) ) ;
#5339 = ADVANCED_FACE ( 'NONE', ( #4088 ), #9102, .T. ) ;
#5340 = VECTOR ( 'NONE', #4169, 1000.000000000000000 ) ;
#5341 = FACE_OUTER_BOUND ( 'NONE', #8462, .T. ) ;
#5342 = DIRECTION ( 'NONE',  ( 0.000000000000000000, 0.000000000000000000, -1.000000000000000000 ) ) ;
#5343 = CARTESIAN_POINT ( 'NONE',  ( -10.35533905932739174, 1.687500000000000000, 24.99999999999999289 ) ) ;
#5344 = LINE ( 'NONE', #10357, #7633 ) ;
#5345 = ORIENTED_EDGE ( 'NONE', *, *, #5954, .F. ) ;
#5346 = ORIENTED_EDGE ( 'NONE', *, *, #6071, .T. ) ;
#5347 = AXIS2_PLACEMENT_3D ( 'NONE', #6533, #5754, #4937 ) ;
#5348 = ORIENTED_EDGE ( 'NONE', *, *, #1157, .F. ) ;
#5349 = CARTESIAN_POINT ( 'NONE',  ( 0.000000000000000000, 85.00000000000000000, -25.00000000000000000 ) ) ;
#5350 = EDGE_CURVE ( 'NONE', #3918, #9337, #5698, .T. ) ;
#5351 = VECTOR ( 'NONE', #8677, 1000.000000000000000 ) ;
#5352 = PLANE ( 'NONE',  #8509 ) ;
#5353 = VERTEX_POINT ( 'NONE', #10711 ) ;
#5354 = FACE_OUTER_BOUND ( 'NONE', #3362, .T. ) ;
#5355 = CIRCLE ( 'NONE', #565, 28.00000000000000000 ) ;
#5356 = DIRECTION ( 'NONE',  ( 0.000000000000000000, 1.000000000000000000, -0.000000000000000000 ) ) ;
#5357 = AXIS2_PLACEMENT_3D ( 'NONE', #5454, #6964, #267 ) ;
#5358 = CARTESIAN_POINT ( 'NONE',  ( 0.000000000000000000, 31.00000000000000000, 0.000000000000000000 ) ) ;
#5359 = LINE ( 'NONE', #8482, #8117 ) ;
#5360 = DIRECTION ( 'NONE',  ( 0.000000000000000000, 0.8660254037844380415, -0.5000000000000009992 ) ) ;
#5361 = CARTESIAN_POINT ( 'NONE',  ( 24.62111388750000174, 5.393749999044085364, 0.000000000000000000 ) ) ;
#5362 = ORIENTED_EDGE ( 'NONE', *, *, #1216, .T. ) ;
#5363 = AXIS2_PLACEMENT_3D ( 'NONE', #6150, #4324, #5821 ) ;
#5364 = EDGE_LOOP ( 'NONE', ( #7918, #4632, #2301, #5375 ) ) ;
#5365 = TOROIDAL_SURFACE ( 'NONE', #6248, 7.399999999999999467, 0.1000000000000000472 ) ;
#5366 = CARTESIAN_POINT ( 'NONE',  ( 0.000000000000000000, 85.00000000000000000, 0.000000000000000000 ) ) ;
#5367 = CARTESIAN_POINT ( 'NONE',  ( -4.592425496802574367E-15, 1.362499998088169129, 25.00000000000000000 ) ) ;
#5368 = CARTESIAN_POINT ( 'NONE',  ( -24.62111388750000174, 2.831249999044084475, -10.19839929293506131 ) ) ;
#5369 = AXIS2_PLACEMENT_3D ( 'NONE', #5220, #8505, #894 ) ;
#5370 = DIRECTION ( 'NONE',  ( 0.3273268353539895426, -0.000000000000000000, 0.9449111825230677164 ) ) ;
#5371 = AXIS2_PLACEMENT_3D ( 'NONE', #6503, #8312, #4134 ) ;
#5372 = DIRECTION ( 'NONE',  ( 0.000000000000000000, 1.000000000000000000, 0.000000000000000000 ) ) ;
#5373 = DIRECTION ( 'NONE',  ( 0.000000000000000000, 0.000000000000000000, -1.000000000000000000 ) ) ;
#5374 = AXIS2_PLACEMENT_3D ( 'NONE', #2463, #8493, #10937 ) ;
#5375 = ORIENTED_EDGE ( 'NONE', *, *, #5200, .F. ) ;
#5376 = CONICAL_SURFACE ( 'NONE', #6076, 25.00000000000000000, 0.3490658503988666728 ) ;
#5377 = VERTEX_POINT ( 'NONE', #5851 ) ;
#5378 = DIRECTION ( 'NONE',  ( 0.000000000000000000, -1.000000000000000000, 0.000000000000000000 ) ) ;
#5379 = VECTOR ( 'NONE', #10270, 1000.000000000000114 ) ;
#5380 = CARTESIAN_POINT ( 'NONE',  ( -25.00000000000001066, 0.5625000000000002220, 10.35533905932737397 ) ) ;
#5381 = CARTESIAN_POINT ( 'NONE',  ( -24.62111388750000884, 0.9562499990440846975, 10.19839929293505421 ) ) ;
#5382 = VERTEX_POINT ( 'NONE', #6687 ) ;
#5383 = CARTESIAN_POINT ( 'NONE',  ( 0.000000000000000000, 10.00000000000000355, 0.000000000000000000 ) ) ;
#5384 = DIRECTION ( 'NONE',  ( 0.000000000000000000, 1.000000000000000000, -0.000000000000000000 ) ) ;
#5385 = CARTESIAN_POINT ( 'NONE',  ( -4.522825247065398226E-15, 2.968749999044084653, 24.62111388750000174 ) ) ;
#5386 = EDGE_CURVE ( 'NONE', #120, #7041, #8383, .T. ) ;
#5387 = DIRECTION ( 'NONE',  ( 0.000000000000000000, 0.000000000000000000, 1.000000000000000000 ) ) ;
#5388 = ORIENTED_EDGE ( 'NONE', *, *, #4182, .F. ) ;
#5389 = EDGE_CURVE ( 'NONE', #8432, #1720, #3284, .T. ) ;
#5390 = LINE ( 'NONE', #5482, #4074 ) ;
#5391 = CARTESIAN_POINT ( 'NONE',  ( 10.19839929293506486, 1.031249999044084653, 24.62111388749999819 ) ) ;
#5392 = CARTESIAN_POINT ( 'NONE',  ( 24.62111388749999463, 4.331249999044085364, 10.19839929293507730 ) ) ;
#5393 = CARTESIAN_POINT ( 'NONE',  ( 1.530808498934191521E-15, 3.862499998088169573, -25.00000000000000000 ) ) ;
#5394 = CARTESIAN_POINT ( 'NONE',  ( 25.00000000000000000, 2.062500000000000000, -10.35533905932737753 ) ) ;
#5395 = EDGE_CURVE ( 'NONE', #2789, #6566, #2335, .T. ) ;
#5396 = EDGE_CURVE ( 'NONE', #6575, #9230, #7520, .T. ) ;
#5397 = CARTESIAN_POINT ( 'NONE',  ( 2.999999999999996447, -0.001000000000001000089, -19.75000000000000000 ) ) ;
#5398 = DIRECTION ( 'NONE',  ( 0.000000000000000000, 0.000000000000000000, 1.000000000000000000 ) ) ;
#5399 = CARTESIAN_POINT ( 'NONE',  ( 0.000000000000000000, 8.000000000000003553, -25.00000000000000000 ) ) ;
#5400 = DIRECTION ( 'NONE',  ( 0.000000000000000000, -1.000000000000000000, 0.000000000000000000 ) ) ;
#5401 = DIRECTION ( 'NONE',  ( 0.000000000000000000, 0.000000000000000000, 1.000000000000000000 ) ) ;
#5402 = EDGE_LOOP ( 'NONE', ( #1918, #9571, #829, #4685, #7758, #1689 ) ) ;
#5403 = ORIENTED_EDGE ( 'NONE', *, *, #8009, .T. ) ;
#5404 = EDGE_CURVE ( 'NONE', #7897, #1247, #606, .T. ) ;
#5405 = ORIENTED_EDGE ( 'NONE', *, *, #9013, .F. ) ;
#5406 = CARTESIAN_POINT ( 'NONE',  ( -18.60400172474273361, 25.00000000000000000, -7.276923788646511682 ) ) ;
#5407 = CYLINDRICAL_SURFACE ( 'NONE', #4821, 22.00000000000000355 ) ;
#5408 = EDGE_CURVE ( 'NONE', #1988, #806, #8510, .T. ) ;
#5409 = DIRECTION ( 'NONE',  ( 0.000000000000000000, 0.000000000000000000, 1.000000000000000000 ) ) ;
#5410 = DIRECTION ( 'NONE',  ( 0.000000000000000000, -0.000000000000000000, 1.000000000000000000 ) ) ;
#5411 = CARTESIAN_POINT ( 'NONE',  ( 24.62111388750000174, 0.2812499990440845976, -10.19839929293505776 ) ) ;
#5412 = DIRECTION ( 'NONE',  ( 0.000000000000000000, 0.000000000000000000, 1.000000000000000000 ) ) ;
#5413 = EDGE_CURVE ( 'NONE', #6661, #5017, #3758, .T. ) ;
#5414 = ORIENTED_EDGE ( 'NONE', *, *, #10369, .F. ) ;
#5415 = CARTESIAN_POINT ( 'NONE',  ( -24.62111388750000884, 3.956249999044084475, 10.19839929293505421 ) ) ;
#5416 = FACE_OUTER_BOUND ( 'NONE', #10473, .T. ) ;
#5417 = FACE_BOUND ( 'NONE', #5943, .T. ) ;
#5418 = PLANE ( 'NONE',  #6410 ) ;
#5419 = DIRECTION ( 'NONE',  ( 0.000000000000000000, 0.000000000000000000, -1.000000000000000000 ) ) ;
#5420 = ORIENTED_EDGE ( 'NONE', *, *, #4788, .T. ) ;
#5421 = ORIENTED_EDGE ( 'NONE', *, *, #3757, .T. ) ;
#5422 = DIRECTION ( 'NONE',  ( -0.000000000000000000, 1.000000000000000000, -0.000000000000000000 ) ) ;
#5423 = CARTESIAN_POINT ( 'NONE',  ( 17.67766952966369232, 3.125000000000000000, -17.67766952966369232 ) ) ;
#5424 = DIRECTION ( 'NONE',  ( -1.000000000000000000, 0.000000000000000000, 0.000000000000000000 ) ) ;
#5425 = ORIENTED_EDGE ( 'NONE', *, *, #8734, .T. ) ;
#5426 = FACE_OUTER_BOUND ( 'NONE', #8844, .T. ) ;
#5427 = LINE ( 'NONE', #6148, #239 ) ;
#5428 = CARTESIAN_POINT ( 'NONE',  ( -10.19839929293507375, 1.906249999044084431, 24.62111388749999108 ) ) ;
#5429 = CARTESIAN_POINT ( 'NONE',  ( 1.530808498934191521E-15, 2.250000000000000444, -25.00000000000000000 ) ) ;
#5430 = ORIENTED_EDGE ( 'NONE', *, *, #2509, .T. ) ;
#5431 = ORIENTED_EDGE ( 'NONE', *, *, #1882, .F. ) ;
#5432 = PRODUCT_DEFINITION ( 'UNKNOWN', '', #347, #4624 ) ;
#5433 = CARTESIAN_POINT ( 'NONE',  ( 24.62111388750000174, 3.218749999044084653, 0.000000000000000000 ) ) ;
#5434 = VECTOR ( 'NONE', #7006, 1000.000000000000000 ) ;
#5435 = CARTESIAN_POINT ( 'NONE',  ( 17.40975659021752620, 3.268749999044084475, 17.40975659021753330 ) ) ;
#5436 = SHAPE_REPRESENTATION ( 'Removable Crank Handle & Arm Unit', ( #7040 ), #6672 ) ;
#5437 = CARTESIAN_POINT ( 'NONE',  ( -25.00000000000000000, 2.500000000000000000, -3.061616997868383043E-15 ) ) ;
#5438 = CARTESIAN_POINT ( 'NONE',  ( -13.63990010960498367, 28.00000000000000000, -7.874999999999870326 ) ) ;
#5439 = LINE ( 'NONE', #4723, #3884 ) ;
#5440 = FACE_BOUND ( 'NONE', #8351, .T. ) ;
#5441 = CARTESIAN_POINT ( 'NONE',  ( 0.000000000000000000, 5.000000000000000000, 0.000000000000000000 ) ) ;
#5442 = VECTOR ( 'NONE', #3608, 1000.000000000000000 ) ;
#5443 = VERTEX_POINT ( 'NONE', #1489 ) ;
#5444 = ORIENTED_EDGE ( 'NONE', *, *, #10019, .F. ) ;
#5445 = ADVANCED_FACE ( 'NONE', ( #7387 ), #5795, .F. ) ;
#5446 = ADVANCED_FACE ( 'NONE', ( #772 ), #9933, .T. ) ;
#5447 = CARTESIAN_POINT ( 'NONE',  ( 25.00000000000000000, 0.6124999980881691286, 0.000000000000000000 ) ) ;
#5448 = TOROIDAL_SURFACE ( 'NONE', #8248, 3.379762621896238883, 2.000000000000000000 ) ;
#5449 = AXIS2_PLACEMENT_3D ( 'NONE', #1893, #895, #8623 ) ;
#5450 = DIRECTION ( 'NONE',  ( -0.000000000000000000, 1.000000000000000000, -0.000000000000000000 ) ) ;
#5451 = ADVANCED_FACE ( 'NONE', ( #4193 ), #9058, .T. ) ;
#5452 = CARTESIAN_POINT ( 'NONE',  ( 5.796693311223892309, 19.03096903053431532, 3.924072712834481447 ) ) ;
#5453 = DIRECTION ( 'NONE',  ( 0.8660254037844362651, 0.000000000000000000, -0.5000000000000041078 ) ) ;
#5454 = CARTESIAN_POINT ( 'NONE',  ( 1.040834085586084257E-14, 90.00000000000001421, 0.000000000000000000 ) ) ;
#5455 = EDGE_CURVE ( 'NONE', #3821, #1673, #6468, .T. ) ;
#5456 = ORIENTED_EDGE ( 'NONE', *, *, #3903, .F. ) ;
#5457 = CARTESIAN_POINT ( 'NONE',  ( 28.09696521099633060, 102.8977774788672264, 5.000000000000000000 ) ) ;
#5458 = PLANE ( 'NONE',  #9865 ) ;
#5459 = EDGE_CURVE ( 'NONE', #8414, #6293, #5637, .T. ) ;
#5460 = CYLINDRICAL_SURFACE ( 'NONE', #8179, 25.00000000000000000 ) ;
#5461 = FACE_OUTER_BOUND ( 'NONE', #4987, .T. ) ;
#5462 = CARTESIAN_POINT ( 'NONE',  ( 2.999999999999999112, 25.00000000000000000, 19.75000000000000000 ) ) ;
#5463 = PRODUCT_DEFINITION_FORMATION_WITH_SPECIFIED_SOURCE ( 'ANY', '', #8820, .NOT_KNOWN. ) ;
#5464 = ORIENTED_EDGE ( 'NONE', *, *, #1331, .T. ) ;
#5465 = ORIENTED_EDGE ( 'NONE', *, *, #10770, .F. ) ;
#5466 = VECTOR ( 'NONE', #10604, 1000.000000000000114 ) ;
#5467 = DIRECTION ( 'NONE',  ( 1.000000000000000000, -0.000000000000000000, -0.000000000000000000 ) ) ;
#5468 = CARTESIAN_POINT ( 'NONE',  ( -10.35533905932738108, 0.6875000000000002220, 24.99999999999999645 ) ) ;
#5469 = VECTOR ( 'NONE', #671, 1000.000000000000000 ) ;
#5470 = CARTESIAN_POINT ( 'NONE',  ( 24.62111388750000174, 1.456249999044084920, -10.19839929293505776 ) ) ;
#5471 = EDGE_CURVE ( 'NONE', #2423, #3051, #9401, .T. ) ;
#5472 = ORIENTED_EDGE ( 'NONE', *, *, #10924, .F. ) ;
#5473 = CARTESIAN_POINT ( 'NONE',  ( 0.1339745962155587111, 10.00000000000000355, 12.92820323027550700 ) ) ;
#5474 = DIRECTION ( 'NONE',  ( 1.000000000000000000, 0.000000000000000000, 0.000000000000000000 ) ) ;
#5475 = CARTESIAN_POINT ( 'NONE',  ( 1.040834085586084257E-14, 88.00000000000001421, 0.000000000000000000 ) ) ;
#5476 = CARTESIAN_POINT ( 'NONE',  ( -10.19839929293507375, 4.906249999044083765, 24.62111388749999108 ) ) ;
#5477 = DIRECTION ( 'NONE',  ( 0.000000000000000000, -1.000000000000000000, 0.000000000000000000 ) ) ;
#5478 = AXIS2_PLACEMENT_3D ( 'NONE', #2083, #432, #2898 ) ;
#5479 = VERTEX_POINT ( 'NONE', #945 ) ;
#5480 = CIRCLE ( 'NONE', #5656, 25.00000000000000000 ) ;
#5481 = VERTEX_POINT ( 'NONE', #103 ) ;
#5482 = CARTESIAN_POINT ( 'NONE',  ( 0.000000000000000000, 85.00000000000000000, -25.00000000000000000 ) ) ;
#5483 = CARTESIAN_POINT ( 'NONE',  ( 24.62111388749999463, 4.156249999044083765, 10.19839929293507730 ) ) ;
#5484 = CARTESIAN_POINT ( 'NONE',  ( 1.507608415688466075E-15, 1.643749999044084475, -24.62111388750000174 ) ) ;
#5485 = ORIENTED_EDGE ( 'NONE', *, *, #3634, .F. ) ;
#5486 = DIRECTION ( 'NONE',  ( 0.000000000000000000, 1.000000000000000000, 0.000000000000000000 ) ) ;
#5487 = FILL_AREA_STYLE_COLOUR ( '', #1915 ) ;
#5488 = VECTOR ( 'NONE', #2158, 1000.000000000000000 ) ;
#5489 = MECHANICAL_DESIGN_GEOMETRIC_PRESENTATION_REPRESENTATION (  '', ( #10251 ), #4447 ) ;
#5490 = DIRECTION ( 'NONE',  ( 0.000000000000000000, 1.000000000000000000, 0.000000000000000000 ) ) ;
#5491 = CARTESIAN_POINT ( 'NONE',  ( 25.00000000000000000, 0.6124999980881691286, 0.000000000000000000 ) ) ;
#5492 = DIRECTION ( 'NONE',  ( 1.000000000000000000, 0.000000000000000000, 0.000000000000000000 ) ) ;
#5493 = DIRECTION ( 'NONE',  ( 0.5000000000000012212, 0.000000000000000000, 0.8660254037844380415 ) ) ;
#5494 = ORIENTED_EDGE ( 'NONE', *, *, #2406, .T. ) ;
#5495 = ORIENTED_EDGE ( 'NONE', *, *, #5189, .T. ) ;
#5496 = VERTEX_POINT ( 'NONE', #1000 ) ;
#5497 = CIRCLE ( 'NONE', #2843, 2.999999999999997780 ) ;
#5498 = FACE_OUTER_BOUND ( 'NONE', #3212, .T. ) ;
#5499 = CYLINDRICAL_SURFACE ( 'NONE', #2187, 25.00000000000000000 ) ;
#5500 = CARTESIAN_POINT ( 'NONE',  ( 0.000000000000000000, 7.000000000000003553, 0.000000000000000000 ) ) ;
#5501 = EDGE_CURVE ( 'NONE', #9763, #8026, #8436, .T. ) ;
#5502 = FACE_OUTER_BOUND ( 'NONE', #1933, .T. ) ;
#5503 = CARTESIAN_POINT ( 'NONE',  ( 0.000000000000000000, 5.000000000000000000, 0.000000000000000000 ) ) ;
#5504 = CIRCLE ( 'NONE', #5682, 2.999999999999997335 ) ;
#5505 = ORIENTED_EDGE ( 'NONE', *, *, #10696, .T. ) ;
#5506 = ORIENTED_EDGE ( 'NONE', *, *, #5333, .T. ) ;
#5507 = VECTOR ( 'NONE', #1121, 1000.000000000000000 ) ;
#5508 = ADVANCED_FACE ( 'NONE', ( #4365 ), #6977, .T. ) ;
#5509 = ORIENTED_EDGE ( 'NONE', *, *, #3895, .T. ) ;
#5510 = CARTESIAN_POINT ( 'NONE',  ( 0.000000000000000000, 5.000000000000000000, 0.000000000000000000 ) ) ;
#5511 = LINE ( 'NONE', #7023, #8285 ) ;
#5512 = DIRECTION ( 'NONE',  ( 0.000000000000000000, 0.000000000000000000, 1.000000000000000000 ) ) ;
#5513 = DIRECTION ( 'NONE',  ( 1.000000000000000000, 0.000000000000000000, 0.000000000000000000 ) ) ;
#5514 = EDGE_CURVE ( 'NONE', #4041, #1319, #9003, .T. ) ;
#5515 = DIRECTION ( 'NONE',  ( 0.000000000000000000, 0.8660254037844380415, 0.5000000000000009992 ) ) ;
#5516 = ADVANCED_FACE ( 'NONE', ( #6850, #5145 ), #4312, .T. ) ;
#5517 = VECTOR ( 'NONE', #5315, 1000.000000000000000 ) ;
#5518 = AXIS2_PLACEMENT_3D ( 'NONE', #7814, #1022, #1728 ) ;
#5519 = ADVANCED_FACE ( 'NONE', ( #2519 ), #2497, .F. ) ;
#5520 = ORIENTED_EDGE ( 'NONE', *, *, #388, .F. ) ;
#5521 = STYLED_ITEM ( 'NONE', ( #3840 ), #7050 ) ;
#5522 = AXIS2_PLACEMENT_3D ( 'NONE', #5949, #4296, #7659 ) ;
#5523 = DIRECTION ( 'NONE',  ( 0.000000000000000000, 0.000000000000000000, 1.000000000000000000 ) ) ;
#5524 = FACE_OUTER_BOUND ( 'NONE', #8453, .T. ) ;
#5525 = CARTESIAN_POINT ( 'NONE',  ( -0.5000000000000000000, 7.781088913245554295, 13.47724133595216323 ) ) ;
#5526 = CARTESIAN_POINT ( 'NONE',  ( -4.522825247065398226E-15, 2.143749999044084920, 24.62111388750000174 ) ) ;
#5527 = EDGE_LOOP ( 'NONE', ( #2095, #8234, #3278, #1284 ) ) ;
#5528 = CARTESIAN_POINT ( 'NONE',  ( 1.500000000000001332, 0.000000000000000000, 0.000000000000000000 ) ) ;
#5529 = FILL_AREA_STYLE ('',( #10550 ) ) ;
#5530 = CARTESIAN_POINT ( 'NONE',  ( 10.35533905932737930, 2.799999998088169573, -25.00000000000000000 ) ) ;
#5531 = ORIENTED_EDGE ( 'NONE', *, *, #1434, .F. ) ;
#5532 = AXIS2_PLACEMENT_3D ( 'NONE', #8940, #9872, #9818 ) ;
#5533 = CARTESIAN_POINT ( 'NONE',  ( 24.62111388749999108, 3.156249999044084653, 10.19839929293507730 ) ) ;
#5534 = CARTESIAN_POINT ( 'NONE',  ( 0.000000000000000000, 0.000000000000000000, 0.000000000000000000 ) ) ;
#5535 = ORIENTED_EDGE ( 'NONE', *, *, #2071, .T. ) ;
#5536 = AXIS2_PLACEMENT_3D ( 'NONE', #5358, #1100, #10422 ) ;
#5537 = EDGE_LOOP ( 'NONE', ( #3649, #819, #6486, #3906, #1245, #1611 ) ) ;
#5538 = ORIENTED_EDGE ( 'NONE', *, *, #8141, .F. ) ;
#5539 = EDGE_CURVE ( 'NONE', #1367, #4397, #7610, .T. ) ;
#5540 = ADVANCED_FACE ( 'NONE', ( #3460 ), #6919, .T. ) ;
#5541 = CIRCLE ( 'NONE', #9228, 25.00000000000000000 ) ;
#5542 = LINE ( 'NONE', #790, #10250 ) ;
#5543 = CARTESIAN_POINT ( 'NONE',  ( -4.522825247065398226E-15, 2.968749999044084653, 24.62111388750000174 ) ) ;
#5544 = CARTESIAN_POINT ( 'NONE',  ( -17.40975659021752975, 2.768749999044084475, -17.40975659021752975 ) ) ;
#5545 = ORIENTED_EDGE ( 'NONE', *, *, #2914, .F. ) ;
#5546 = VECTOR ( 'NONE', #4736, 1000.000000000000000 ) ;
#5547 = CARTESIAN_POINT ( 'NONE',  ( 10.35533905932737930, 3.187500000000000000, -25.00000000000000000 ) ) ;
#5548 = DIRECTION ( 'NONE',  ( 0.000000000000000000, 1.000000000000000000, 0.000000000000000000 ) ) ;
#5549 = CARTESIAN_POINT ( 'NONE',  ( 1.530808498934191521E-15, 1.862499998088169129, -25.00000000000000000 ) ) ;
#5550 = DIRECTION ( 'NONE',  ( -0.000000000000000000, 1.000000000000000000, -0.000000000000000000 ) ) ;
#5551 = FACE_OUTER_BOUND ( 'NONE', #7586, .T. ) ;
#5552 = EDGE_CURVE ( 'NONE', #2139, #292, #6798, .T. ) ;
#5553 = VERTEX_POINT ( 'NONE', #9504 ) ;
#5554 = EDGE_LOOP ( 'NONE', ( #3742, #6982, #8728, #3008 ) ) ;
#5555 = ORIENTED_EDGE ( 'NONE', *, *, #6141, .F. ) ;
#5556 = ORIENTED_EDGE ( 'NONE', *, *, #7042, .T. ) ;
#5557 = CARTESIAN_POINT ( 'NONE',  ( -3.058047309050066165, 19.03096903053433309, 6.296693311223885203 ) ) ;
#5558 = DIRECTION ( 'NONE',  ( -1.000000000000000000, 0.000000000000000000, 0.000000000000000000 ) ) ;
#5559 = CARTESIAN_POINT ( 'NONE',  ( 6.386751345948143310, 10.00000000000000355, -11.06217782649107839 ) ) ;
#5560 = CARTESIAN_POINT ( 'NONE',  ( 0.000000000000000000, 31.00000000000000000, -10.50000000000000000 ) ) ;
#5561 = CARTESIAN_POINT ( 'NONE',  ( -0.4330127018922172999, 0.000000000000000000, -0.2500000000000036082 ) ) ;
#5562 = PLANE ( 'NONE',  #2997 ) ;
#5563 = CARTESIAN_POINT ( 'NONE',  ( -2.999999999999999112, 28.00000000000000000, -19.75000000000000000 ) ) ;
#5564 =( BOUNDED_CURVE ( )  B_SPLINE_CURVE ( 2, ( #1415, #9091, #5733, #2450, #4904, #3061, #10651, #1520, #4021 ),
 .UNSPECIFIED., .F., .F. ) 
 B_SPLINE_CURVE_WITH_KNOTS ( ( 3, 2, 2, 2, 3 ),
 ( 0.1500000000000000222, 0.1750000000000000167, 0.2000000000000000389, 0.2250000000000000333, 0.2500000000000000000 ),
 .UNSPECIFIED. ) 
 CURVE ( )  GEOMETRIC_REPRESENTATION_ITEM ( )  RATIONAL_B_SPLINE_CURVE ( ( 0.9999999999999998890, 0.9238795325112868495, 1.000000000000000000, 0.9238795325112867385, 1.000000000000000000, 0.9238795325112867385, 1.000000000000000000, 0.9238795325112867385, 1.000000000000000000 ) ) 
 REPRESENTATION_ITEM ( '' )  );
#5565 = ORIENTED_EDGE ( 'NONE', *, *, #5037, .T. ) ;
#5566 = VERTEX_POINT ( 'NONE', #9258 ) ;
#5567 = EDGE_LOOP ( 'NONE', ( #7417, #1632, #1993, #7883 ) ) ;
#5568 = DIRECTION ( 'NONE',  ( -0.000000000000000000, -1.000000000000000000, -0.000000000000000000 ) ) ;
#5569 = CARTESIAN_POINT ( 'NONE',  ( 25.00000000000000000, 0.6749999980881691286, -10.35533905932737753 ) ) ;
#5570 = CARTESIAN_POINT ( 'NONE',  ( 10.35533905932738286, 4.424999998088169129, 24.99999999999999645 ) ) ;
#5571 = DIRECTION ( 'NONE',  ( 0.9185586535436925937, 0.3535533905932736198, -0.1767766952966332017 ) ) ;
#5572 = CARTESIAN_POINT ( 'NONE',  ( 82.32050807568876394, 92.28203230275514102, -4.000000000000006217 ) ) ;
#5573 = ORIENTED_EDGE ( 'NONE', *, *, #9025, .T. ) ;
#5574 = ADVANCED_FACE ( 'NONE', ( #2569 ), #10940, .T. ) ;
#5575 = EDGE_CURVE ( 'NONE', #5443, #4321, #3382, .T. ) ;
#5576 = EDGE_CURVE ( 'NONE', #1857, #5785, #3585, .T. ) ;
#5577 =( LENGTH_UNIT ( ) NAMED_UNIT ( * ) SI_UNIT ( .MILLI., .METRE. ) );
#5578 = CARTESIAN_POINT ( 'NONE',  ( 25.52691073765301510, 98.96446609406727646, 5.000000000000000000 ) ) ;
#5579 = CARTESIAN_POINT ( 'NONE',  ( 1.507608415688466075E-15, 3.643749999044084920, -24.62111388750000174 ) ) ;
#5580 = ORIENTED_EDGE ( 'NONE', *, *, #9560, .F. ) ;
#5581 = FACE_OUTER_BOUND ( 'NONE', #1033, .T. ) ;
#5582 = FILL_AREA_STYLE_COLOUR ( '', #10186 ) ;
#5583 = CARTESIAN_POINT ( 'NONE',  ( 6.994037468151971915, 19.34316356887878641, -0.3335819196118459673 ) ) ;
#5584 = CARTESIAN_POINT ( 'NONE',  ( 24.62111388750000174, 3.281249999044084653, -10.19839929293505776 ) ) ;
#5585 = DIRECTION ( 'NONE',  ( -0.000000000000000000, 1.000000000000000000, -0.000000000000000000 ) ) ;
#5586 = EDGE_CURVE ( 'NONE', #416, #9664, #8671, .T. ) ;
#5587 = ORIENTED_EDGE ( 'NONE', *, *, #10113, .F. ) ;
#5588 = ORIENTED_EDGE ( 'NONE', *, *, #26, .T. ) ;
#5589 = ORIENTED_EDGE ( 'NONE', *, *, #533, .F. ) ;
#5590 = EDGE_CURVE ( 'NONE', #5068, #10398, #2502, .T. ) ;
#5591 = CARTESIAN_POINT ( 'NONE',  ( 17.40975659021752975, 0.5187499990440845865, -17.40975659021752975 ) ) ;
#5592 = CARTESIAN_POINT ( 'NONE',  ( -6.580127018922051541, 10.00000000000000355, -11.12916512459894314 ) ) ;
#5593 = CARTESIAN_POINT ( 'NONE',  ( -10.19839929293507552, 2.081249999044084475, 24.62111388749999463 ) ) ;
#5594 = ORIENTED_EDGE ( 'NONE', *, *, #3895, .F. ) ;
#5595 = CARTESIAN_POINT ( 'NONE',  ( -25.00000000000001421, 1.562500000000000000, 10.35533905932737397 ) ) ;
#5596 = PLANE ( 'NONE',  #2591 ) ;
#5597 = CARTESIAN_POINT ( 'NONE',  ( -1.500000000000000444, 83.00000000000000000, -1.500000000000000222 ) ) ;
#5598 = FACE_OUTER_BOUND ( 'NONE', #4555, .T. ) ;
#5599 = CARTESIAN_POINT ( 'NONE',  ( 17.67766952966368521, 3.487499998088169129, 17.67766952966369232 ) ) ;
#5600 = EDGE_CURVE ( 'NONE', #7830, #10741, #9758, .T. ) ;
#5601 = MECHANICAL_DESIGN_GEOMETRIC_PRESENTATION_REPRESENTATION (  '', ( #1360 ), #8410 ) ;
#5602 = EDGE_LOOP ( 'NONE', ( #7158, #7068, #10231, #2260 ) ) ;
#5603 = ORIENTED_EDGE ( 'NONE', *, *, #1525, .T. ) ;
#5604 = ORIENTED_EDGE ( 'NONE', *, *, #9215, .F. ) ;
#5605 = ORIENTED_EDGE ( 'NONE', *, *, #7749, .F. ) ;
#5606 = UNCERTAINTY_MEASURE_WITH_UNIT (LENGTH_MEASURE( 1.000000000000000082E-05 ), #352, 'distance_accuracy_value', 'NONE');
#5607 = CARTESIAN_POINT ( 'NONE',  ( 0.000000000000000000, 0.000000000000000000, 0.000000000000000000 ) ) ;
#5608 = CARTESIAN_POINT ( 'NONE',  ( -17.67766952966369232, 4.625000000000000000, 17.67766952966368876 ) ) ;
#5609 = COLOUR_RGB ( '', 0.09019608, 0.27058824, 0.51372549) ;
#5610 = CARTESIAN_POINT ( 'NONE',  ( -9.874999999999777955, -0.001000000000001000089, 20.10400172474279401 ) ) ;
#5611 = DIRECTION ( 'NONE',  ( 0.000000000000000000, 1.000000000000000000, 0.000000000000000000 ) ) ;
#5612 = AXIS2_PLACEMENT_3D ( 'NONE', #7710, #2774, #4409 ) ;
#5613 = LINE ( 'NONE', #2185, #1593 ) ;
#5614 = DIRECTION ( 'NONE',  ( -0.000000000000000000, 1.000000000000000000, -0.000000000000000000 ) ) ;
#5615 = ORIENTED_EDGE ( 'NONE', *, *, #4302, .F. ) ;
#5616 = ORIENTED_EDGE ( 'NONE', *, *, #658, .F. ) ;
#5617 = CIRCLE ( 'NONE', #4581, 2.999999999999998224 ) ;
#5618 = ORIENTED_EDGE ( 'NONE', *, *, #6894, .T. ) ;
#5619 = ORIENTED_EDGE ( 'NONE', *, *, #8980, .F. ) ;
#5620 = VECTOR ( 'NONE', #8018, 1000.000000000000114 ) ;
#5621 = DIRECTION ( 'NONE',  ( 0.000000000000000000, 0.000000000000000000, 1.000000000000000000 ) ) ;
#5622 = CARTESIAN_POINT ( 'NONE',  ( 0.000000000000000000, 5.000000000000000000, 0.000000000000000000 ) ) ;
#5623 = FACE_OUTER_BOUND ( 'NONE', #7560, .T. ) ;
#5624 =( BOUNDED_CURVE ( )  B_SPLINE_CURVE ( 2, ( #1148, #1795, #7927, #7053, #10408, #2826, #6225, #6827, #9587 ),
 .UNSPECIFIED., .F., .F. ) 
 B_SPLINE_CURVE_WITH_KNOTS ( ( 3, 2, 2, 2, 3 ),
 ( 0.4500000000000000111, 0.4749999999999999778, 0.5000000000000000000, 0.5250000000000000222, 0.5500000000000000444 ),
 .UNSPECIFIED. ) 
 CURVE ( )  GEOMETRIC_REPRESENTATION_ITEM ( )  RATIONAL_B_SPLINE_CURVE ( ( 1.000000000000000000, 0.9238795325112867385, 1.000000000000000000, 0.9238795325112867385, 1.000000000000000000, 0.9238795325112867385, 1.000000000000000000, 0.9238795325112867385, 1.000000000000000000 ) ) 
 REPRESENTATION_ITEM ( '' )  );
#5625 = CARTESIAN_POINT ( 'NONE',  ( -10.00000000000000000, 93.00000000000001421, 5.000000000000000000 ) ) ;
#5626 = CARTESIAN_POINT ( 'NONE',  ( 5.812177826491076615, 10.00000000000000355, -3.933012701892204532 ) ) ;
#5627 = VECTOR ( 'NONE', #8319, 1000.000000000000000 ) ;
#5628 = EDGE_LOOP ( 'NONE', ( #477, #9641, #5804, #5892 ) ) ;
#5629 = ORIENTED_EDGE ( 'NONE', *, *, #8262, .T. ) ;
#5630 = DIRECTION ( 'NONE',  ( -0.000000000000000000, -1.000000000000000000, -0.000000000000000000 ) ) ;
#5631 = SURFACE_SIDE_STYLE ('',( #2245 ) ) ;
#5632 = CARTESIAN_POINT ( 'NONE',  ( 17.40975659021752620, 4.268749999044084475, 17.40975659021753330 ) ) ;
#5633 = ADVANCED_FACE ( 'NONE', ( #1316 ), #10593, .T. ) ;
#5634 = ORIENTED_EDGE ( 'NONE', *, *, #1380, .T. ) ;
#5635 = CARTESIAN_POINT ( 'NONE',  ( 25.00000000000000000, 3.674999998088170017, -10.35533905932737753 ) ) ;
#5636 = EDGE_LOOP ( 'NONE', ( #6609, #9864, #656, #3753 ) ) ;
#5637 = LINE ( 'NONE', #1425, #3203 ) ;
#5638 = CARTESIAN_POINT ( 'NONE',  ( 10.19839929293505953, 3.406249999044085097, -24.62111388750000174 ) ) ;
#5639 = AXIS2_PLACEMENT_3D ( 'NONE', #654, #4974, #7384 ) ;
#5640 = EDGE_CURVE ( 'NONE', #4321, #9229, #1996, .T. ) ;
#5641 = ORIENTED_EDGE ( 'NONE', *, *, #5275, .T. ) ;
#5642 = ORIENTED_EDGE ( 'NONE', *, *, #5986, .F. ) ;
#5643 = CIRCLE ( 'NONE', #879, 5.999999999999999112 ) ;
#5644 = AXIS2_PLACEMENT_3D ( 'NONE', #726, #3358, #4107 ) ;
#5645 = ADVANCED_FACE ( 'NONE', ( #3006 ), #7950, .T. ) ;
#5646 = CARTESIAN_POINT ( 'NONE',  ( -25.00000000000000000, 4.112499998088169129, -3.061616997868383043E-15 ) ) ;
#5647 = DIRECTION ( 'NONE',  ( 0.4999999999999947820, 0.000000000000000000, -0.8660254037844417052 ) ) ;
#5648 = CARTESIAN_POINT ( 'NONE',  ( -10.19839929293505776, 2.531249999044085097, -24.62111388750000174 ) ) ;
#5649 = ORIENTED_EDGE ( 'NONE', *, *, #6227, .F. ) ;
#5650 = PLANE ( 'NONE',  #1261 ) ;
#5651 = CARTESIAN_POINT ( 'NONE',  ( -6.145599950363623165, 19.66631150450993815, 3.355508642977428124 ) ) ;
#5652 = FACE_OUTER_BOUND ( 'NONE', #6527, .T. ) ;
#5653 = DIRECTION ( 'NONE',  ( 0.000000000000000000, -0.000000000000000000, 1.000000000000000000 ) ) ;
#5654 = CARTESIAN_POINT ( 'NONE',  ( 8.660254037844401509, 95.00000000000001421, 5.000000000000000000 ) ) ;
#5655 = CIRCLE ( 'NONE', #884, 2.999999999999997335 ) ;
#5656 = AXIS2_PLACEMENT_3D ( 'NONE', #1543, #2316, #4043 ) ;
#5657 = ADVANCED_FACE ( 'NONE', ( #7128 ), #5418, .T. ) ;
#5658 = ORIENTED_EDGE ( 'NONE', *, *, #9019, .F. ) ;
#5659 = ORIENTED_EDGE ( 'NONE', *, *, #1576, .F. ) ;
#5660 = ORIENTED_EDGE ( 'NONE', *, *, #5051, .F. ) ;
#5661 = EDGE_CURVE ( 'NONE', #10861, #9966, #4495, .T. ) ;
#5662 = VECTOR ( 'NONE', #4673, 999.9999999999998863 ) ;
#5663 = AXIS2_PLACEMENT_3D ( 'NONE', #10378, #9553, #7306 ) ;
#5664 = DIRECTION ( 'NONE',  ( 0.000000000000000000, -1.000000000000000000, 0.000000000000000000 ) ) ;
#5665 = CARTESIAN_POINT ( 'NONE',  ( -17.10400172474254532, 28.00000000000000000, 12.87500000000020250 ) ) ;
#5666 = DIRECTION ( 'NONE',  ( 0.000000000000000000, -2.775557561562888270E-17, -1.000000000000000000 ) ) ;
#5667 = FACE_OUTER_BOUND ( 'NONE', #5874, .T. ) ;
#5668 = CARTESIAN_POINT ( 'NONE',  ( 10.19839929293506486, 4.031249999044083765, 24.62111388749999819 ) ) ;
#5669 = DIRECTION ( 'NONE',  ( 0.000000000000000000, 0.000000000000000000, -1.000000000000000000 ) ) ;
#5670 = CIRCLE ( 'NONE', #8480, 2.999999999999998668 ) ;
#5671 = ORIENTED_EDGE ( 'NONE', *, *, #5413, .T. ) ;
#5672 = ADVANCED_FACE ( 'NONE', ( #5461 ), #380, .F. ) ;
#5673 = ORIENTED_EDGE ( 'NONE', *, *, #6268, .T. ) ;
#5674 = ORIENTED_EDGE ( 'NONE', *, *, #646, .T. ) ;
#5675 = CYLINDRICAL_SURFACE ( 'NONE', #8858, 30.00000000000000000 ) ;
#5676 = CARTESIAN_POINT ( 'NONE',  ( -3.785909150703094195, 19.34316356887878285, 5.890223162633836829 ) ) ;
#5677 = DIRECTION ( 'NONE',  ( -0.000000000000000000, -0.000000000000000000, 1.000000000000000000 ) ) ;
#5678 = AXIS2_PLACEMENT_3D ( 'NONE', #3495, #7761, #4462 ) ;
#5679 = LINE ( 'NONE', #6670, #2346 ) ;
#5680 = PLANE ( 'NONE',  #225 ) ;
#5681 = ORIENTED_EDGE ( 'NONE', *, *, #5200, .T. ) ;
#5682 = AXIS2_PLACEMENT_3D ( 'NONE', #6102, #896, #2706 ) ;
#5683 = CARTESIAN_POINT ( 'NONE',  ( 0.000000000000000000, 28.00000000000000000, 0.000000000000000000 ) ) ;
#5684 = DIRECTION ( 'NONE',  ( -0.000000000000000000, 1.000000000000000000, -0.000000000000000000 ) ) ;
#5685 = CARTESIAN_POINT ( 'NONE',  ( 18.60400172474268032, 28.00000000000000000, 7.276923788646640467 ) ) ;
#5686 = CARTESIAN_POINT ( 'NONE',  ( -17.40975659021752975, 2.768749999044084475, -17.40975659021752975 ) ) ;
#5687 = ORIENTED_EDGE ( 'NONE', *, *, #9624, .F. ) ;
#5688 = CIRCLE ( 'NONE', #9196, 4.500000000000000888 ) ;
#5689 = CARTESIAN_POINT ( 'NONE',  ( 28.02691073765301155, 94.63433907514509258, 5.000000000000000000 ) ) ;
#5690 = APPLICATION_PROTOCOL_DEFINITION ( 'draft international standard', 'automotive_design', 1998, #5756 ) ;
#5691 = DIRECTION ( 'NONE',  ( 0.000000000000000000, 0.000000000000000000, 1.000000000000000000 ) ) ;
#5692 = CARTESIAN_POINT ( 'NONE',  ( -17.67766952966368876, 1.375000000000000000, -17.67766952966369232 ) ) ;
#5693 = CARTESIAN_POINT ( 'NONE',  ( -24.62111388750000174, 0.7187499990440845421, -3.015216831376932151E-15 ) ) ;
#5694 = AXIS2_PLACEMENT_3D ( 'NONE', #313, #4478, #5194 ) ;
#5695 = VERTEX_POINT ( 'NONE', #7906 ) ;
#5696 = ORIENTED_EDGE ( 'NONE', *, *, #8198, .F. ) ;
#5697 = AXIS2_PLACEMENT_3D ( 'NONE', #5776, #9087, #10811 ) ;
#5698 = CIRCLE ( 'NONE', #6579, 25.00000000000000000 ) ;
#5699 = CARTESIAN_POINT ( 'NONE',  ( -24.62111388750000174, 0.8937499990440845865, -3.015216831376932151E-15 ) ) ;
#5700 = CARTESIAN_POINT ( 'NONE',  ( -0.5000000000000000000, 10.00000000000000355, 6.982120021884467675 ) ) ;
#5701 = AXIS2_PLACEMENT_3D ( 'NONE', #8412, #9186, #1625 ) ;
#5702 = CARTESIAN_POINT ( 'NONE',  ( -24.62111388750000174, 3.718749999044084653, -3.015216831376932151E-15 ) ) ;
#5703 = ORIENTED_EDGE ( 'NONE', *, *, #4452, .T. ) ;
#5704 = EDGE_CURVE ( 'NONE', #9703, #4100, #8732, .T. ) ;
#5705 = CARTESIAN_POINT ( 'NONE',  ( 0.1668442477450398642, 19.66631150450990617, -6.999999999999997335 ) ) ;
#5706 = DIRECTION ( 'NONE',  ( 0.000000000000000000, 0.000000000000000000, -1.000000000000000000 ) ) ;
#5707 = VECTOR ( 'NONE', #1549, 1000.000000000000000 ) ;
#5708 = DIRECTION ( 'NONE',  ( 0.000000000000000000, -2.775557561562891351E-17, -1.000000000000000000 ) ) ;
#5709 = DIRECTION ( 'NONE',  ( -0.1889822365046156527, -0.000000000000000000, 0.9819805060619652970 ) ) ;
#5710 = DIRECTION ( 'NONE',  ( -1.000000000000000000, 0.000000000000000000, 0.000000000000000000 ) ) ;
#5711 = CARTESIAN_POINT ( 'NONE',  ( 2.999999999999998224, 25.00000000000000000, 15.75000000000000355 ) ) ;
#5712 = EDGE_CURVE ( 'NONE', #9230, #6463, #2136, .T. ) ;
#5713 = VERTEX_POINT ( 'NONE', #10539 ) ;
#5714 = VERTEX_POINT ( 'NONE', #2950 ) ;
#5715 = UNCERTAINTY_MEASURE_WITH_UNIT (LENGTH_MEASURE( 1.000000000000000082E-05 ), #1890, 'distance_accuracy_value', 'NONE');
#5716 = EDGE_CURVE ( 'NONE', #1227, #2972, #2871, .T. ) ;
#5717 = EDGE_CURVE ( 'NONE', #8432, #2098, #7220, .T. ) ;
#5718 = CARTESIAN_POINT ( 'NONE',  ( 24.62111388750000174, 1.218749999044084431, 0.000000000000000000 ) ) ;
#5719 = DIRECTION ( 'NONE',  ( 0.000000000000000000, 0.000000000000000000, 1.000000000000000000 ) ) ;
#5720 = AXIS2_PLACEMENT_3D ( 'NONE', #2501, #5898, #9247 ) ;
#5721 = CARTESIAN_POINT ( 'NONE',  ( 0.000000000000000000, 10.00000000000000355, 0.000000000000000000 ) ) ;
#5722 = CARTESIAN_POINT ( 'NONE',  ( -4.522825247065398226E-15, 2.968749999044084653, 24.62111388750000174 ) ) ;
#5723 = CARTESIAN_POINT ( 'NONE',  ( 2.716379529800028356E-15, -1.026060429977008193, 22.18092213764227694 ) ) ;
#5724 = ADVANCED_FACE ( 'NONE', ( #10437 ), #10477, .T. ) ;
#5725 = VERTEX_POINT ( 'NONE', #4700 ) ;
#5726 = VERTEX_POINT ( 'NONE', #9710 ) ;
#5727 = EDGE_LOOP ( 'NONE', ( #8545, #5946, #8317, #1533 ) ) ;
#5728 = ORIENTED_EDGE ( 'NONE', *, *, #10024, .T. ) ;
#5729 = ADVANCED_FACE ( 'NONE', ( #3695 ), #6254, .T. ) ;
#5730 = DIRECTION ( 'NONE',  ( -0.8660254037844327124, 0.000000000000000000, 0.5000000000000103251 ) ) ;
#5731 = CARTESIAN_POINT ( 'NONE',  ( -3.500000000000049294, 20.00000000000000355, 6.062177826491040200 ) ) ;
#5732 = DIRECTION ( 'NONE',  ( 0.000000000000000000, 1.000000000000000000, 0.000000000000000000 ) ) ;
#5733 = CARTESIAN_POINT ( 'NONE',  ( 17.67766952966368521, 0.8750000000000000000, 17.67766952966369232 ) ) ;
#5734 = DIRECTION ( 'NONE',  ( 0.000000000000000000, 1.000000000000000000, 0.000000000000000000 ) ) ;
#5735 = EDGE_CURVE ( 'NONE', #5067, #2931, #1131, .T. ) ;
#5736 = EDGE_LOOP ( 'NONE', ( #4923, #6873, #9965, #10173 ) ) ;
#5737 = PRESENTATION_STYLE_ASSIGNMENT (( #2359 ) ) ;
#5738 = LINE ( 'NONE', #8107, #5264 ) ;
#5739 = CARTESIAN_POINT ( 'NONE',  ( -24.62111388750000884, 4.956249999044084475, 10.19839929293505421 ) ) ;
#5740 = ORIENTED_EDGE ( 'NONE', *, *, #4167, .F. ) ;
#5741 = CARTESIAN_POINT ( 'NONE',  ( 10.35533905932738286, 3.424999998088169129, 24.99999999999999645 ) ) ;
#5742 = CARTESIAN_POINT ( 'NONE',  ( -4.592425496802574367E-15, 2.362499998088169129, 25.00000000000000000 ) ) ;
#5743 = DIRECTION ( 'NONE',  ( -1.000000000000000000, 0.000000000000000000, 0.000000000000000000 ) ) ;
#5744 = CARTESIAN_POINT ( 'NONE',  ( 17.40975659021752975, 2.343749999044085097, -17.40975659021752975 ) ) ;
#5745 = VERTEX_POINT ( 'NONE', #9659 ) ;
#5746 = CARTESIAN_POINT ( 'NONE',  ( -10.35533905932737575, 2.924999998088168685, -25.00000000000000000 ) ) ;
#5747 = DIRECTION ( 'NONE',  ( 0.9449111825230630535, -0.000000000000000000, 0.3273268353540027542 ) ) ;
#5748 = CARTESIAN_POINT ( 'NONE',  ( 10.19839929293506486, 2.031249999044084653, 24.62111388749999819 ) ) ;
#5749 = ORIENTED_EDGE ( 'NONE', *, *, #3973, .T. ) ;
#5750 = LINE ( 'NONE', #9833, #2113 ) ;
#5751 =( NAMED_UNIT ( * ) PLANE_ANGLE_UNIT ( ) SI_UNIT ( $, .RADIAN. ) );
#5752 = DIRECTION ( 'NONE',  ( 0.000000000000000000, 1.000000000000000000, 0.000000000000000000 ) ) ;
#5753 = DIRECTION ( 'NONE',  ( 1.000000000000000000, 0.000000000000000000, 0.000000000000000000 ) ) ;
#5754 = DIRECTION ( 'NONE',  ( -0.000000000000000000, -1.000000000000000000, -0.000000000000000000 ) ) ;
#5755 = CARTESIAN_POINT ( 'NONE',  ( 3.061616997868383043E-15, 85.00000000000000000, 25.00000000000000000 ) ) ;
#5756 = APPLICATION_CONTEXT ( 'automotive_design' ) ;
#5757 = EDGE_LOOP ( 'NONE', ( #2493, #3600, #9801, #7693, #3321 ) ) ;
#5758 = CARTESIAN_POINT ( 'NONE',  ( 24.62111388750000174, 2.456249999044084475, -10.19839929293505776 ) ) ;
#5759 = DIRECTION ( 'NONE',  ( 0.000000000000000000, 0.000000000000000000, -1.000000000000000000 ) ) ;
#5760 = DIRECTION ( 'NONE',  ( -1.000000000000000000, 0.000000000000000000, 0.000000000000000000 ) ) ;
#5761 = VERTEX_POINT ( 'NONE', #2851 ) ;
#5762 = CARTESIAN_POINT ( 'NONE',  ( 3.500000000000004885, 20.00000000000000355, -6.062177826491062405 ) ) ;
#5763 = CARTESIAN_POINT ( 'NONE',  ( -24.62111388750000884, 0.7812499990440845421, 10.19839929293505421 ) ) ;
#5764 = CARTESIAN_POINT ( 'NONE',  ( 7.874999999999916511, 28.00000000000000000, -13.63990010960495702 ) ) ;
#5765 = CARTESIAN_POINT ( 'NONE',  ( 10.19839929293506486, 2.031249999044084653, 24.62111388749999819 ) ) ;
#5766 = DIRECTION ( 'NONE',  ( 0.000000000000000000, -2.775557561562891351E-17, -1.000000000000000000 ) ) ;
#5767 = ORIENTED_EDGE ( 'NONE', *, *, #3696, .T. ) ;
#5768 = EDGE_CURVE ( 'NONE', #4764, #6575, #5564, .T. ) ;
#5769 = ORIENTED_EDGE ( 'NONE', *, *, #10458, .T. ) ;
#5770 = VERTEX_POINT ( 'NONE', #5835 ) ;
#5771 = EDGE_CURVE ( 'NONE', #457, #9729, #7465, .T. ) ;
#5772 = ORIENTED_EDGE ( 'NONE', *, *, #9277, .F. ) ;
#5773 = CIRCLE ( 'NONE', #2935, 5.000000000000004441 ) ;
#5774 = EDGE_CURVE ( 'NONE', #10429, #8432, #6956, .T. ) ;
#5775 = VECTOR ( 'NONE', #6210, 1000.000000000000000 ) ;
#5776 = CARTESIAN_POINT ( 'NONE',  ( -11.42163336986822308, 7.781088913245559624, -7.171633369868438912 ) ) ;
#5777 =( BOUNDED_CURVE ( )  B_SPLINE_CURVE ( 2, ( #1050, #7667, #157, #97, #3455 ),
 .UNSPECIFIED., .F., .F. ) 
 B_SPLINE_CURVE_WITH_KNOTS ( ( 3, 2, 3 ),
 ( 0.9500000000000000666, 0.9750000000000000888, 1.000000000000000000 ),
 .UNSPECIFIED. ) 
 CURVE ( )  GEOMETRIC_REPRESENTATION_ITEM ( )  RATIONAL_B_SPLINE_CURVE ( ( 0.9999999999999996669, 0.9238795325112870716, 1.000000000000000000, 0.9238795325112867385, 1.000000000000000000 ) ) 
 REPRESENTATION_ITEM ( '' )  );
#5778 = CARTESIAN_POINT ( 'NONE',  ( 82.32050807568876394, 92.28203230275514102, 0.000000000000000000 ) ) ;
#5779 = CARTESIAN_POINT ( 'NONE',  ( 82.32050807568876394, 102.2820323027551410, -3.379762621896238883 ) ) ;
#5780 = CYLINDRICAL_SURFACE ( 'NONE', #2506, 2.149999999999999911 ) ;
#5781 = CARTESIAN_POINT ( 'NONE',  ( 14.02827699982873888, 5.000000000000000888, 20.42037923990229942 ) ) ;
#5782 = ADVANCED_FACE ( 'NONE', ( #7373 ), #8100, .T. ) ;
#5783 = AXIS2_PLACEMENT_3D ( 'NONE', #6112, #4278, #6881 ) ;
#5784 = VERTEX_POINT ( 'NONE', #8255 ) ;
#5785 = VERTEX_POINT ( 'NONE', #1476 ) ;
#5786 = EDGE_CURVE ( 'NONE', #9491, #7766, #10028, .T. ) ;
#5787 = SURFACE_SIDE_STYLE ('',( #702 ) ) ;
#5788 = DIRECTION ( 'NONE',  ( 0.000000000000000000, 0.000000000000000000, -1.000000000000000000 ) ) ;
#5789 = ORIENTED_EDGE ( 'NONE', *, *, #3481, .T. ) ;
#5790 = LINE ( 'NONE', #3071, #9161 ) ;
#5791 = SHAPE_DEFINITION_REPRESENTATION ( #2896, #6555 ) ;
#5792 = DIRECTION ( 'NONE',  ( 0.000000000000000000, 0.000000000000000000, -1.000000000000000000 ) ) ;
#5793 = VERTEX_POINT ( 'NONE', #4077 ) ;
#5794 = AXIS2_PLACEMENT_3D ( 'NONE', #5205, #2510, #1756 ) ;
#5795 = PLANE ( 'NONE',  #7452 ) ;
#5796 = CARTESIAN_POINT ( 'NONE',  ( -10.19839929293505776, 0.5312499990440845421, -24.62111388750000174 ) ) ;
#5797 = ORIENTED_EDGE ( 'NONE', *, *, #7474, .F. ) ;
#5798 = ORIENTED_EDGE ( 'NONE', *, *, #5716, .T. ) ;
#5799 = EDGE_CURVE ( 'NONE', #2242, #2252, #5148, .T. ) ;
#5800 = CARTESIAN_POINT ( 'NONE',  ( -17.40975659021753330, 1.018749999044084698, 17.40975659021752975 ) ) ;
#5801 = CARTESIAN_POINT ( 'NONE',  ( 1.530808498934191521E-15, 3.862499998088169573, -25.00000000000000000 ) ) ;
#5802 = CARTESIAN_POINT ( 'NONE',  ( -24.62111388750000884, 1.781249999044084431, 10.19839929293505421 ) ) ;
#5803 = DIRECTION ( 'NONE',  ( 0.000000000000000000, -2.775557561562888270E-17, -1.000000000000000000 ) ) ;
#5804 = ORIENTED_EDGE ( 'NONE', *, *, #2410, .F. ) ;
#5805 = DIRECTION ( 'NONE',  ( 0.000000000000000000, 0.000000000000000000, -1.000000000000000000 ) ) ;
#5806 = FILL_AREA_STYLE ('',( #2320 ) ) ;
#5807 = FILL_AREA_STYLE ('',( #8280 ) ) ;
#5808 = DIRECTION ( 'NONE',  ( -0.000000000000000000, 1.000000000000000000, -0.000000000000000000 ) ) ;
#5809 = CARTESIAN_POINT ( 'NONE',  ( 3.673940397442059178E-15, 88.00000000000001421, 30.00000000000000000 ) ) ;
#5810 = PLANE ( 'NONE',  #8683 ) ;
#5811 = PLANE ( 'NONE',  #2979 ) ;
#5812 = VERTEX_POINT ( 'NONE', #3218 ) ;
#5813 = ORIENTED_EDGE ( 'NONE', *, *, #4473, .T. ) ;
#5814 = CARTESIAN_POINT ( 'NONE',  ( 10.35533905932738286, 5.424999998088169129, 24.99999999999999645 ) ) ;
#5815 = FACE_OUTER_BOUND ( 'NONE', #5602, .T. ) ;
#5816 = AXIS2_PLACEMENT_3D ( 'NONE', #378, #10537, #277 ) ;
#5817 = AXIS2_PLACEMENT_3D ( 'NONE', #8228, #5753, #8282 ) ;
#5818 = ORIENTED_EDGE ( 'NONE', *, *, #2347, .F. ) ;
#5819 = ADVANCED_FACE ( 'NONE', ( #6456 ), #5780, .F. ) ;
#5820 = LINE ( 'NONE', #12, #6712 ) ;
#5821 = DIRECTION ( 'NONE',  ( 0.000000000000000000, 0.000000000000000000, 1.000000000000000000 ) ) ;
#5822 = LINE ( 'NONE', #1734, #1801 ) ;
#5823 = CARTESIAN_POINT ( 'NONE',  ( -17.40975659021753330, 0.8437499990440846531, 17.40975659021752975 ) ) ;
#5824 = DIRECTION ( 'NONE',  ( 0.000000000000000000, -1.000000000000000000, 2.775557561562888270E-17 ) ) ;
#5825 = ORIENTED_EDGE ( 'NONE', *, *, #6080, .T. ) ;
#5826 = ORIENTED_EDGE ( 'NONE', *, *, #5189, .F. ) ;
#5827 = AXIS2_PLACEMENT_3D ( 'NONE', #3510, #9488, #4539 ) ;
#5828 = CIRCLE ( 'NONE', #8990, 5.000000000000000000 ) ;
#5829 = VERTEX_POINT ( 'NONE', #8984 ) ;
#5830 = PLANE ( 'NONE',  #8323 ) ;
#5831 = EDGE_CURVE ( 'NONE', #6402, #1429, #3655, .T. ) ;
#5832 = DIRECTION ( 'NONE',  ( -2.168404344971010594E-16, 0.000000000000000000, -1.000000000000000000 ) ) ;
#5833 = VECTOR ( 'NONE', #8187, 1000.000000000000114 ) ;
#5834 = AXIS2_PLACEMENT_3D ( 'NONE', #3397, #10876, #1645 ) ;
#5835 = CARTESIAN_POINT ( 'NONE',  ( -15.13990010960484867, 28.00000000000000000, 5.276923788646865177 ) ) ;
#5836 = DIRECTION ( 'NONE',  ( 0.000000000000000000, -1.000000000000000000, 0.000000000000000000 ) ) ;
#5837 = EDGE_CURVE ( 'NONE', #7237, #5856, #3945, .T. ) ;
#5838 = VERTEX_POINT ( 'NONE', #9144 ) ;
#5839 =( BOUNDED_CURVE ( )  B_SPLINE_CURVE ( 2, ( #5367, #274, #7307, #8726, #1168, #1108, #1399, #10735, #10630 ),
 .UNSPECIFIED., .F., .F. ) 
 B_SPLINE_CURVE_WITH_KNOTS ( ( 3, 2, 2, 2, 3 ),
 ( 0.1499999999999999944, 0.1749999999999999889, 0.2000000000000000111, 0.2249999999999999778, 0.2499999999999999722 ),
 .UNSPECIFIED. ) 
 CURVE ( )  GEOMETRIC_REPRESENTATION_ITEM ( )  RATIONAL_B_SPLINE_CURVE ( ( 1.000000000000000000, 0.9238795325112867385, 1.000000000000000000, 0.9238795325112867385, 1.000000000000000000, 0.9238795325112867385, 1.000000000000000000, 0.9238795325112868495, 0.9999999999999998890 ) ) 
 REPRESENTATION_ITEM ( '' )  );
#5840 = CARTESIAN_POINT ( 'NONE',  ( 15.75000000000001421, 25.00000000000000000, 2.999999999999942268 ) ) ;
#5841 = DIRECTION ( 'NONE',  ( 0.000000000000000000, 0.000000000000000000, -1.000000000000000000 ) ) ;
#5842 = CARTESIAN_POINT ( 'NONE',  ( 10.81217782649105708, 10.00000000000000355, 5.665063509461154112 ) ) ;
#5843 = VECTOR ( 'NONE', #2026, 1000.000000000000000 ) ;
#5844 = CARTESIAN_POINT ( 'NONE',  ( -5.796693311223946488, 19.03096903053430466, 3.924072712834398846 ) ) ;
#5845 = ORIENTED_EDGE ( 'NONE', *, *, #10086, .T. ) ;
#5846 = EDGE_CURVE ( 'NONE', #2468, #7557, #5679, .T. ) ;
#5847 = DIRECTION ( 'NONE',  ( -0.8660254037844328234, 0.000000000000000000, -0.5000000000000101030 ) ) ;
#5848 = APPLICATION_PROTOCOL_DEFINITION ( 'draft international standard', 'automotive_design', 1998, #673 ) ;
#5849 = EDGE_CURVE ( 'NONE', #5164, #1247, #583, .T. ) ;
#5850 = DIRECTION ( 'NONE',  ( -0.000000000000000000, -1.000000000000000000, -0.000000000000000000 ) ) ;
#5851 = CARTESIAN_POINT ( 'NONE',  ( 0.000000000000000000, 31.00000000000000000, -7.500000000000000888 ) ) ;
#5852 = CARTESIAN_POINT ( 'NONE',  ( 17.40975659021752620, 2.093749999044084653, 17.40975659021753330 ) ) ;
#5853 = ADVANCED_FACE ( 'NONE', ( #3163, #2354 ), #6559, .T. ) ;
#5854 = EDGE_LOOP ( 'NONE', ( #2275, #6281, #5494, #10457 ) ) ;
#5855 = VECTOR ( 'NONE', #7349, 1000.000000000000000 ) ;
#5856 = VERTEX_POINT ( 'NONE', #4236 ) ;
#5857 = VECTOR ( 'NONE', #6206, 1000.000000000000000 ) ;
#5858 = CARTESIAN_POINT ( 'NONE',  ( -24.62111388750000174, 3.831249999044084920, -10.19839929293506131 ) ) ;
#5859 = CARTESIAN_POINT ( 'NONE',  ( -7.875000000000116351, -0.001000000000001000089, -10.63990010960484511 ) ) ;
#5860 = CARTESIAN_POINT ( 'NONE',  ( 24.62111388749999463, 3.156249999044084653, 10.19839929293507730 ) ) ;
#5861 = CARTESIAN_POINT ( 'NONE',  ( -10.00000000000000000, 90.00000000000001421, -5.000000000000000000 ) ) ;
#5862 = VERTEX_POINT ( 'NONE', #2614 ) ;
#5863 = ADVANCED_FACE ( 'NONE', ( #10320 ), #1638, .T. ) ;
#5864 = DIRECTION ( 'NONE',  ( 0.000000000000000000, 0.000000000000000000, -1.000000000000000000 ) ) ;
#5865 = DIRECTION ( 'NONE',  ( 1.000000000000000000, 0.000000000000000000, 0.000000000000000000 ) ) ;
#5866 = AXIS2_PLACEMENT_3D ( 'NONE', #2893, #3738, #5304 ) ;
#5867 = CARTESIAN_POINT ( 'NONE',  ( 9.184850993605149917E-16, 28.00000000000000000, 7.500000000000000888 ) ) ;
#5868 = CARTESIAN_POINT ( 'NONE',  ( 1.500000000000001332, 8.299669118052623479E-16, 5.525000000000000355 ) ) ;
#5869 = CARTESIAN_POINT ( 'NONE',  ( 2.449293598294706414E-16, 25.00000000000000355, 2.000000000000000000 ) ) ;
#5870 = EDGE_CURVE ( 'NONE', #492, #2, #10108, .T. ) ;
#5871 = VECTOR ( 'NONE', #146, 1000.000000000000000 ) ;
#5872 = VECTOR ( 'NONE', #8298, 1000.000000000000000 ) ;
#5873 = EDGE_CURVE ( 'NONE', #5829, #9988, #10926, .T. ) ;
#5874 = EDGE_LOOP ( 'NONE', ( #3444, #4361, #9148 ) ) ;
#5875 = ORIENTED_EDGE ( 'NONE', *, *, #1522, .T. ) ;
#5876 = ORIENTED_EDGE ( 'NONE', *, *, #10242, .T. ) ;
#5877 = CIRCLE ( 'NONE', #8705, 30.00000000000000000 ) ;
#5878 = FACE_OUTER_BOUND ( 'NONE', #6599, .T. ) ;
#5879 = CARTESIAN_POINT ( 'NONE',  ( 17.40975659021752620, 3.268749999044084475, 17.40975659021753330 ) ) ;
#5880 = AXIS2_PLACEMENT_3D ( 'NONE', #2181, #3733, #7932 ) ;
#5881 = CARTESIAN_POINT ( 'NONE',  ( -24.62111388750000174, 1.718749999044084431, -3.015216831376932151E-15 ) ) ;
#5882 = AXIS2_PLACEMENT_3D ( 'NONE', #6196, #280, #8882 ) ;
#5883 = CARTESIAN_POINT ( 'NONE',  ( -19.39162934935757931, 5.000000000000000888, 15.17115553405142947 ) ) ;
#5884 = CARTESIAN_POINT ( 'NONE',  ( -4.592425496802574367E-15, 4.362499998088169129, 25.00000000000000000 ) ) ;
#5885 = EDGE_CURVE ( 'NONE', #795, #7692, #9412, .T. ) ;
#5886 = ADVANCED_FACE ( 'NONE', ( #90 ), #8539, .T. ) ;
#5887 = CARTESIAN_POINT ( 'NONE',  ( 1.507608415688466075E-15, 3.468749999044085097, -24.62111388750000174 ) ) ;
#5888 = DIRECTION ( 'NONE',  ( 0.000000000000000000, 0.000000000000000000, -1.000000000000000000 ) ) ;
#5889 = ORIENTED_EDGE ( 'NONE', *, *, #6791, .T. ) ;
#5890 = VERTEX_POINT ( 'NONE', #9305 ) ;
#5891 = VECTOR ( 'NONE', #8764, 999.9999999999998863 ) ;
#5892 = ORIENTED_EDGE ( 'NONE', *, *, #3385, .F. ) ;
#5893 = VERTEX_POINT ( 'NONE', #9248 ) ;
#5894 = EDGE_LOOP ( 'NONE', ( #4014, #1130, #6370, #1594 ) ) ;
#5895 = AXIS2_PLACEMENT_3D ( 'NONE', #6975, #8607, #4646 ) ;
#5896 = DIRECTION ( 'NONE',  ( -3.491481338843133355E-15, 0.000000000000000000, 1.000000000000000000 ) ) ;
#5897 = CARTESIAN_POINT ( 'NONE',  ( 2.500000000000000444, 1.000000000000001998, 0.5773502691896277295 ) ) ;
#5898 = DIRECTION ( 'NONE',  ( 0.000000000000000000, 1.000000000000000000, 0.000000000000000000 ) ) ;
#5899 = DIRECTION ( 'NONE',  ( 0.4330127018922207971, -0.8660254037844380415, -0.2499999999999995282 ) ) ;
#5900 = CARTESIAN_POINT ( 'NONE',  ( -3.223142256880076948E-15, 25.00000000000000000, -12.75000000000000178 ) ) ;
#5901 = ORIENTED_EDGE ( 'NONE', *, *, #10113, .T. ) ;
#5902 = DIRECTION ( 'NONE',  ( 0.000000000000000000, 0.000000000000000000, 1.000000000000000000 ) ) ;
#5903 = DIRECTION ( 'NONE',  ( 0.000000000000000000, -1.000000000000000000, 0.000000000000000000 ) ) ;
#5904 = DIRECTION ( 'NONE',  ( 0.000000000000000000, 0.000000000000000000, -1.000000000000000000 ) ) ;
#5905 = CARTESIAN_POINT ( 'NONE',  ( 12.19615242270663735, 10.00000000000000355, -0.4999999999999575340 ) ) ;
#5906 = ORIENTED_EDGE ( 'NONE', *, *, #6772, .T. ) ;
#5907 = CARTESIAN_POINT ( 'NONE',  ( 0.000000000000000000, 20.00000000000000355, -2.000000000000000000 ) ) ;
#5908 = DIRECTION ( 'NONE',  ( 1.000000000000000000, 0.000000000000000000, 0.000000000000000000 ) ) ;
#5909 = CARTESIAN_POINT ( 'NONE',  ( 0.000000000000000000, 25.00000000000000355, 0.000000000000000000 ) ) ;
#5910 = CARTESIAN_POINT ( 'NONE',  ( 0.000000000000000000, 85.00000000000000000, 0.000000000000000000 ) ) ;
#5911 = ORIENTED_EDGE ( 'NONE', *, *, #4096, .T. ) ;
#5912 = ADVANCED_FACE ( 'NONE', ( #3388 ), #6252, .F. ) ;
#5913 =( BOUNDED_CURVE ( )  B_SPLINE_CURVE ( 2, ( #5884, #4219, #9238, #5938, #6655, #912, #4281, #10015, #2439 ),
 .UNSPECIFIED., .F., .F. ) 
 B_SPLINE_CURVE_WITH_KNOTS ( ( 3, 2, 2, 2, 3 ),
 ( 0.7500000000000000000, 0.7750000000000000222, 0.8000000000000000444, 0.8250000000000000666, 0.8500000000000000888 ),
 .UNSPECIFIED. ) 
 CURVE ( )  GEOMETRIC_REPRESENTATION_ITEM ( )  RATIONAL_B_SPLINE_CURVE ( ( 1.000000000000000000, 0.9238795325112867385, 1.000000000000000000, 0.9238795325112867385, 1.000000000000000000, 0.9238795325112867385, 1.000000000000000000, 0.9238795325112864054, 1.000000000000000444 ) ) 
 REPRESENTATION_ITEM ( '' )  );
#5914 = EDGE_CURVE ( 'NONE', #10217, #3157, #10257, .T. ) ;
#5915 = CARTESIAN_POINT ( 'NONE',  ( -24.62111388750000174, 3.893749999044084475, -3.015216831376932151E-15 ) ) ;
#5916 = CARTESIAN_POINT ( 'NONE',  ( -5.000000000000000000, 93.00000000000001421, -5.000000000000000000 ) ) ;
#5917 = DIRECTION ( 'NONE',  ( -0.000000000000000000, 1.000000000000000000, -0.000000000000000000 ) ) ;
#5918 = FACE_OUTER_BOUND ( 'NONE', #4188, .T. ) ;
#5919 = ORIENTED_EDGE ( 'NONE', *, *, #3893, .T. ) ;
#5920 = LINE ( 'NONE', #8621, #2833 ) ;
#5921 = ADVANCED_FACE ( 'NONE', ( #10144 ), #6838, .T. ) ;
#5922 = DIRECTION ( 'NONE',  ( 1.000000000000000000, 0.000000000000000000, 0.000000000000000000 ) ) ;
#5923 = CARTESIAN_POINT ( 'NONE',  ( 25.00000000000000000, 0.6124999980881691286, 0.000000000000000000 ) ) ;
#5924 = CARTESIAN_POINT ( 'NONE',  ( -0.5000000000000000000, 7.781088913245555183, -13.47724133595216500 ) ) ;
#5925 = DIRECTION ( 'NONE',  ( 1.049727191138620421E-16, -0.5150380749100518241, 0.8571673007021137769 ) ) ;
#5926 = ORIENTED_EDGE ( 'NONE', *, *, #5227, .F. ) ;
#5927 = EDGE_CURVE ( 'NONE', #2102, #2070, #3327, .T. ) ;
#5928 = ORIENTED_EDGE ( 'NONE', *, *, #8553, .F. ) ;
#5929 = UNCERTAINTY_MEASURE_WITH_UNIT (LENGTH_MEASURE( 1.000000000000000082E-05 ), #9834, 'distance_accuracy_value', 'NONE');
#5930 = DIRECTION ( 'NONE',  ( -1.000000000000000000, 0.000000000000000000, 0.000000000000000000 ) ) ;
#5931 = ADVANCED_FACE ( 'NONE', ( #6073 ), #866, .F. ) ;
#5932 = CARTESIAN_POINT ( 'NONE',  ( 24.62111388750000174, 3.456249999044084920, -10.19839929293505776 ) ) ;
#5933 = CARTESIAN_POINT ( 'NONE',  ( -24.62111388750000884, 1.956249999044084475, 10.19839929293505421 ) ) ;
#5934 = CARTESIAN_POINT ( 'NONE',  ( -10.35533905932739174, 0.6875000000000000000, 24.99999999999999289 ) ) ;
#5935 = ADVANCED_FACE ( 'NONE', ( #149 ), #9432, .F. ) ;
#5936 = VERTEX_POINT ( 'NONE', #5127 ) ;
#5937 = CARTESIAN_POINT ( 'NONE',  ( -1.500000000000000444, 88.00000000000001421, -1.500000000000000222 ) ) ;
#5938 = CARTESIAN_POINT ( 'NONE',  ( 24.99999999999999289, 4.549999998088169129, 10.35533905932739529 ) ) ;
#5939 = CARTESIAN_POINT ( 'NONE',  ( -10.35533905932737575, 0.3125000000000000000, -25.00000000000000000 ) ) ;
#5940 = DIRECTION ( 'NONE',  ( 0.000000000000000000, -1.000000000000000000, 0.000000000000000000 ) ) ;
#5941 = VERTEX_POINT ( 'NONE', #8481 ) ;
#5942 = EDGE_LOOP ( 'NONE', ( #6372, #4955, #4174, #1836 ) ) ;
#5943 = EDGE_LOOP ( 'NONE', ( #2227, #10087 ) ) ;
#5944 = CARTESIAN_POINT ( 'NONE',  ( 1.530808498934191521E-15, 2.862499998088169573, -25.00000000000000000 ) ) ;
#5945 = DIRECTION ( 'NONE',  ( 0.8660254037844434816, 0.000000000000000000, 0.4999999999999918399 ) ) ;
#5946 = ORIENTED_EDGE ( 'NONE', *, *, #398, .T. ) ;
#5947 = CARTESIAN_POINT ( 'NONE',  ( 25.00000000000000000, 2.000000000000000000, 0.000000000000000000 ) ) ;
#5948 = CARTESIAN_POINT ( 'NONE',  ( 1.500000000000001332, -1.873501354054951662E-16, -6.750000000000007994 ) ) ;
#5949 = CARTESIAN_POINT ( 'NONE',  ( -12.47307621135344391, -0.001000000000001000089, -15.60400172474256131 ) ) ;
#5950 = FACE_OUTER_BOUND ( 'NONE', #965, .T. ) ;
#5951 = LINE ( 'NONE', #92, #3377 ) ;
#5952 = EDGE_LOOP ( 'NONE', ( #4387, #10714, #4467, #4303, #2220 ) ) ;
#5953 = CLOSED_SHELL ( 'NONE', ( #6598, #7172, #10910, #8544, #8762, #32, #4905, #7690, #5007 ) ) ;
#5954 = EDGE_CURVE ( 'NONE', #564, #10864, #3447, .T. ) ;
#5955 = DIRECTION ( 'NONE',  ( 0.000000000000000000, -1.000000000000000000, 2.775557561562888270E-17 ) ) ;
#5956 = DIRECTION ( 'NONE',  ( -0.000000000000000000, 1.000000000000000000, -0.000000000000000000 ) ) ;
#5957 = CARTESIAN_POINT ( 'NONE',  ( -20.63749999999999574, 0.000000000000000000, 0.000000000000000000 ) ) ;
#5958 = PLANE ( 'NONE',  #7616 ) ;
#5959 = EDGE_LOOP ( 'NONE', ( #6721, #7807, #783, #3482 ) ) ;
#5960 = DIRECTION ( 'NONE',  ( 1.000000000000000000, 0.000000000000000000, 0.000000000000000000 ) ) ;
#5961 = ITEM_DEFINED_TRANSFORMATION ( 'NONE', 'NONE', #9692,  #7040 ) ;
#5962 = FACE_BOUND ( 'NONE', #4715, .T. ) ;
#5963 = VECTOR ( 'NONE', #9767, 999.9999999999998863 ) ;
#5964 = DIRECTION ( 'NONE',  ( 0.000000000000000000, -2.775557561562888270E-17, -1.000000000000000000 ) ) ;
#5965 = CARTESIAN_POINT ( 'NONE',  ( 0.000000000000000000, 31.00000000000000000, 0.000000000000000000 ) ) ;
#5966 = VECTOR ( 'NONE', #4157, 1000.000000000000000 ) ;
#5967 = ORIENTED_EDGE ( 'NONE', *, *, #2451, .F. ) ;
#5968 = VERTEX_POINT ( 'NONE', #3509 ) ;
#5969 = CARTESIAN_POINT ( 'NONE',  ( 24.62111388750000174, 0.4562499990440845865, -10.19839929293505776 ) ) ;
#5970 = CARTESIAN_POINT ( 'NONE',  ( -10.19839929293505776, 3.706249999044084920, -24.62111388750000174 ) ) ;
#5971 = DIRECTION ( 'NONE',  ( 1.000000000000000000, 0.000000000000000000, 0.000000000000000000 ) ) ;
#5972 = CIRCLE ( 'NONE', #4403, 2.999999999999997335 ) ;
#5973 = DIRECTION ( 'NONE',  ( -0.3061862178478914065, -0.3535533905932741194, -0.8838834764831863255 ) ) ;
#5974 = LINE ( 'NONE', #4201, #1116 ) ;
#5975 = ORIENTED_EDGE ( 'NONE', *, *, #2086, .F. ) ;
#5976 = CARTESIAN_POINT ( 'NONE',  ( 0.000000000000000000, 10.10000000000000497, -4.500000000000000888 ) ) ;
#5977 = DIRECTION ( 'NONE',  ( 1.000000000000000000, 0.000000000000000000, 0.000000000000000000 ) ) ;
#5978 = EDGE_CURVE ( 'NONE', #8502, #5893, #1866, .T. ) ;
#5979 = CARTESIAN_POINT ( 'NONE',  ( 25.00000000000000000, 1.612499998088169351, 0.000000000000000000 ) ) ;
#5980 = DIRECTION ( 'NONE',  ( -1.000000000000000000, -0.000000000000000000, -7.228014483236695816E-17 ) ) ;
#5981 = DIRECTION ( 'NONE',  ( 0.000000000000000000, -1.000000000000000000, 0.000000000000000000 ) ) ;
#5982 =( BOUNDED_CURVE ( )  B_SPLINE_CURVE ( 2, ( #234, #2701, #10219, #1947, #3532, #6751, #7801, #7741, #5154 ),
 .UNSPECIFIED., .F., .F. ) 
 B_SPLINE_CURVE_WITH_KNOTS ( ( 3, 2, 2, 2, 3 ),
 ( 0.05000000000000000278, 0.07499999999999999722, 0.1000000000000000056, 0.1250000000000000000, 0.1499999999999999944 ),
 .UNSPECIFIED. ) 
 CURVE ( )  GEOMETRIC_REPRESENTATION_ITEM ( )  RATIONAL_B_SPLINE_CURVE ( ( 1.000000000000000000, 0.9238795325112867385, 1.000000000000000000, 0.9238795325112867385, 1.000000000000000000, 0.9238795325112867385, 1.000000000000000000, 0.9238795325112867385, 1.000000000000000000 ) ) 
 REPRESENTATION_ITEM ( '' )  );
#5983 = AXIS2_PLACEMENT_3D ( 'NONE', #968, #3485, #10460 ) ;
#5984 = ORIENTED_EDGE ( 'NONE', *, *, #10507, .F. ) ;
#5985 = ORIENTED_EDGE ( 'NONE', *, *, #6957, .F. ) ;
#5986 = EDGE_CURVE ( 'NONE', #849, #4742, #1303, .T. ) ;
#5987 = DIRECTION ( 'NONE',  ( 0.000000000000000000, -2.775557561562891351E-17, -1.000000000000000000 ) ) ;
#5988 = CARTESIAN_POINT ( 'NONE',  ( -17.40975659021752975, 3.768749999044084475, -17.40975659021752975 ) ) ;
#5989 = CARTESIAN_POINT ( 'NONE',  ( 24.62111388750000174, 0.3937499990440845865, 0.000000000000000000 ) ) ;
#5990 = CARTESIAN_POINT ( 'NONE',  ( -10.19839929293505776, 1.706249999044084698, -24.62111388750000174 ) ) ;
#5991 = CARTESIAN_POINT ( 'NONE',  ( 1.507608415688466075E-15, 3.468749999044085097, -24.62111388750000174 ) ) ;
#5992 = FACE_OUTER_BOUND ( 'NONE', #612, .T. ) ;
#5993 = EDGE_CURVE ( 'NONE', #3078, #1567, #2694, .T. ) ;
#5994 = PLANE ( 'NONE',  #5783 ) ;
#5995 = CARTESIAN_POINT ( 'NONE',  ( 2.668943309558227117, 5.000000000000000888, 24.58125138907406537 ) ) ;
#5996 = CARTESIAN_POINT ( 'NONE',  ( -0.5590169943749458970, -1.595945597898662527E-16, -5.750000000000006217 ) ) ;
#5997 = CARTESIAN_POINT ( 'NONE',  ( -4.522825247065398226E-15, 4.968749999044083765, 24.62111388750000174 ) ) ;
#5998 = CARTESIAN_POINT ( 'NONE',  ( 0.5000000000000000000, 7.781088913245554295, -13.47724133595216323 ) ) ;
#5999 = VERTEX_POINT ( 'NONE', #7064 ) ;
#6000 = ORIENTED_EDGE ( 'NONE', *, *, #2856, .F. ) ;
#6001 = VERTEX_POINT ( 'NONE', #265 ) ;
#6002 = ADVANCED_FACE ( 'NONE', ( #4538 ), #2782, .T. ) ;
#6003 = DIRECTION ( 'NONE',  ( 1.156482317317872514E-15, 0.000000000000000000, 1.000000000000000000 ) ) ;
#6004 = AXIS2_PLACEMENT_3D ( 'NONE', #6224, #4524, #5398 ) ;
#6005 = CARTESIAN_POINT ( 'NONE',  ( -25.00000000000000000, 4.049999998088169129, -10.35533905932738108 ) ) ;
#6006 = EDGE_LOOP ( 'NONE', ( #5185, #3116, #4347, #4293 ) ) ;
#6007 = DIRECTION ( 'NONE',  ( 0.000000000000000000, -1.000000000000000000, 0.000000000000000000 ) ) ;
#6008 = PLANE ( 'NONE',  #595 ) ;
#6009 = DIRECTION ( 'NONE',  ( 0.000000000000000000, 1.000000000000000000, 0.000000000000000000 ) ) ;
#6010 = FACE_OUTER_BOUND ( 'NONE', #5078, .T. ) ;
#6011 = DIRECTION ( 'NONE',  ( -0.000000000000000000, -1.000000000000000000, -0.000000000000000000 ) ) ;
#6012 = VECTOR ( 'NONE', #2909, 1000.000000000000000 ) ;
#6013 = VECTOR ( 'NONE', #385, 1000.000000000000000 ) ;
#6014 = EDGE_CURVE ( 'NONE', #1658, #6236, #10302, .T. ) ;
#6015 = ORIENTED_EDGE ( 'NONE', *, *, #4702, .T. ) ;
#6016 = EDGE_LOOP ( 'NONE', ( #6355, #6789, #9420, #3541 ) ) ;
#6017 = AXIS2_PLACEMENT_3D ( 'NONE', #8595, #7065, #10199 ) ;
#6018 = DIRECTION ( 'NONE',  ( -0.000000000000000000, 1.000000000000000000, -0.000000000000000000 ) ) ;
#6019 = CYLINDRICAL_SURFACE ( 'NONE', #6200, 4.999999999999997335 ) ;
#6020 = CARTESIAN_POINT ( 'NONE',  ( -17.67766952966369232, 4.625000000000000000, 17.67766952966368876 ) ) ;
#6021 = PRESENTATION_LAYER_ASSIGNMENT (  '', '', ( #7787 ) ) ;
#6022 = CARTESIAN_POINT ( 'NONE',  ( 24.62111388750000174, 4.393749999044084475, 0.000000000000000000 ) ) ;
#6023 = DIRECTION ( 'NONE',  ( 0.4999999999999887312, 0.000000000000000000, -0.8660254037844451469 ) ) ;
#6024 = CYLINDRICAL_SURFACE ( 'NONE', #5374, 6.975000000000008527 ) ;
#6025 = DIRECTION ( 'NONE',  ( -0.000000000000000000, 1.000000000000000000, -0.000000000000000000 ) ) ;
#6026 = CARTESIAN_POINT ( 'NONE',  ( -10.19839929293507375, 4.906249999044083765, 24.62111388749999108 ) ) ;
#6027 = AXIS2_PLACEMENT_3D ( 'NONE', #8031, #8131, #3944 ) ;
#6028 = CARTESIAN_POINT ( 'NONE',  ( 24.62111388750000174, 1.456249999044084475, -10.19839929293505776 ) ) ;
#6029 = CARTESIAN_POINT ( 'NONE',  ( -24.62111388750000174, 1.893749999044084475, -3.015216831376932151E-15 ) ) ;
#6030 = CARTESIAN_POINT ( 'NONE',  ( -2.999999999999997335, 25.00000000000000000, 15.75000000000000355 ) ) ;
#6031 = CARTESIAN_POINT ( 'NONE',  ( 0.000000000000000000, 85.00000000000000000, -25.00000000000000000 ) ) ;
#6032 = LINE ( 'NONE', #5861, #6561 ) ;
#6033 = ORIENTED_EDGE ( 'NONE', *, *, #4093, .T. ) ;
#6034 = CARTESIAN_POINT ( 'NONE',  ( 0.000000000000000000, 5.000000000000000000, 0.000000000000000000 ) ) ;
#6035 = CARTESIAN_POINT ( 'NONE',  ( -1.400000000000001910, 0.000000000000000000, 0.000000000000000000 ) ) ;
#6036 = CARTESIAN_POINT ( 'NONE',  ( 11.16025403784440329, 90.66987298107783033, 5.000000000000000000 ) ) ;
#6037 = CARTESIAN_POINT ( 'NONE',  ( 24.99999999999999289, 2.549999998088169129, 10.35533905932739529 ) ) ;
#6038 = CARTESIAN_POINT ( 'NONE',  ( -1.500000000000000444, 83.00000000000000000, 1.499999999999999778 ) ) ;
#6039 = CARTESIAN_POINT ( 'NONE',  ( -10.35533905932739174, 2.687500000000000888, 24.99999999999999289 ) ) ;
#6040 = CIRCLE ( 'NONE', #3368, 2.999999999999997780 ) ;
#6041 = ORIENTED_EDGE ( 'NONE', *, *, #8492, .T. ) ;
#6042 = EDGE_LOOP ( 'NONE', ( #9537, #2358, #2644, #6319 ) ) ;
#6043 = CIRCLE ( 'NONE', #1278, 0.1000000000000002554 ) ;
#6044 = VERTEX_POINT ( 'NONE', #8655 ) ;
#6045 = DIRECTION ( 'NONE',  ( -0.000000000000000000, 1.000000000000000000, -0.000000000000000000 ) ) ;
#6046 = CARTESIAN_POINT ( 'NONE',  ( 1.507608415688466075E-15, 2.643749999044084920, -24.62111388750000174 ) ) ;
#6047 = VECTOR ( 'NONE', #7312, 1000.000000000000000 ) ;
#6048 = LINE ( 'NONE', #6161, #3030 ) ;
#6049 = CARTESIAN_POINT ( 'NONE',  ( 17.67766952966368521, 4.487499998088169129, 17.67766952966369232 ) ) ;
#6050 = CARTESIAN_POINT ( 'NONE',  ( -10.35533905932737575, 0.3125000000000000000, -25.00000000000000000 ) ) ;
#6051 = ORIENTED_EDGE ( 'NONE', *, *, #1541, .F. ) ;
#6052 = FACE_OUTER_BOUND ( 'NONE', #6898, .T. ) ;
#6053 = FACE_BOUND ( 'NONE', #4811, .T. ) ;
#6054 = FACE_OUTER_BOUND ( 'NONE', #5959, .T. ) ;
#6055 = CARTESIAN_POINT ( 'NONE',  ( 7.856406460551036197, 98.00000000000001421, -5.000000000000000000 ) ) ;
#6056 = CARTESIAN_POINT ( 'NONE',  ( 6.531088913245547189, 10.00000000000000355, -10.31217782649106240 ) ) ;
#6057 = AXIS2_PLACEMENT_3D ( 'NONE', #3625, #5300, #4349 ) ;
#6058 = VERTEX_POINT ( 'NONE', #6125 ) ;
#6059 = CIRCLE ( 'NONE', #2681, 10.50000000000000000 ) ;
#6060 = ORIENTED_EDGE ( 'NONE', *, *, #3846, .F. ) ;
#6061 = EDGE_CURVE ( 'NONE', #9255, #7282, #9544, .T. ) ;
#6062 = ORIENTED_EDGE ( 'NONE', *, *, #7325, .F. ) ;
#6063 = EDGE_CURVE ( 'NONE', #10316, #8829, #8336, .T. ) ;
#6064 = CIRCLE ( 'NONE', #9750, 6.999999999999997335 ) ;
#6065 = DIRECTION ( 'NONE',  ( -1.000000000000000000, 0.000000000000000000, 0.000000000000000000 ) ) ;
#6066 = ADVANCED_FACE ( 'NONE', ( #2838 ), #9487, .T. ) ;
#6067 = AXIS2_PLACEMENT_3D ( 'NONE', #7443, #8216, #4871 ) ;
#6068 = AXIS2_PLACEMENT_3D ( 'NONE', #8043, #1404, #475 ) ;
#6069 = CARTESIAN_POINT ( 'NONE',  ( 13.63990010960487353, 28.00000000000000000, -7.875000000000067502 ) ) ;
#6070 = CARTESIAN_POINT ( 'NONE',  ( -1.500000000000000444, 88.00000000000001421, -1.500000000000000222 ) ) ;
#6071 = EDGE_CURVE ( 'NONE', #8219, #1642, #5006, .T. ) ;
#6072 = CARTESIAN_POINT ( 'NONE',  ( -5.978755702618506085, 19.66631150450992394, -3.644491357022579425 ) ) ;
#6073 = FACE_OUTER_BOUND ( 'NONE', #7997, .T. ) ;
#6074 = CARTESIAN_POINT ( 'NONE',  ( 6.296693311223896750, 19.03096903053431177, 3.058047309050043960 ) ) ;
#6075 = CYLINDRICAL_SURFACE ( 'NONE', #5357, 4.999999999999987566 ) ;
#6076 = AXIS2_PLACEMENT_3D ( 'NONE', #4856, #6405, #7371 ) ;
#6077 = CARTESIAN_POINT ( 'NONE',  ( 10.19839929293505953, 4.581249999044083587, -24.62111388750000174 ) ) ;
#6078 = EDGE_LOOP ( 'NONE', ( #3053, #5531, #2314, #1626 ) ) ;
#6079 = CIRCLE ( 'NONE', #5532, 5.999999999999999112 ) ;
#6080 = EDGE_CURVE ( 'NONE', #7345, #3125, #6414, .T. ) ;
#6081 = ORIENTED_EDGE ( 'NONE', *, *, #26, .F. ) ;
#6082 = AXIS2_PLACEMENT_3D ( 'NONE', #8040, #1307, #6545 ) ;
#6083 = LINE ( 'NONE', #9441, #6913 ) ;
#6084 = FACE_OUTER_BOUND ( 'NONE', #4000, .T. ) ;
#6085 = CARTESIAN_POINT ( 'NONE',  ( 10.19839929293506486, 2.206249999044084920, 24.62111388749999819 ) ) ;
#6086 = DIRECTION ( 'NONE',  ( 1.000000000000000000, 0.000000000000000000, -3.708321773340234242E-15 ) ) ;
#6087 = ADVANCED_FACE ( 'NONE', ( #833 ), #2473, .F. ) ;
#6088 = DIRECTION ( 'NONE',  ( 0.000000000000000000, 0.000000000000000000, 1.000000000000000000 ) ) ;
#6089 = DIRECTION ( 'NONE',  ( 0.000000000000000000, 1.000000000000000000, 0.000000000000000000 ) ) ;
#6090 = CARTESIAN_POINT ( 'NONE',  ( 24.62111388750000174, 4.281249999044084653, -10.19839929293505776 ) ) ;
#6091 = CARTESIAN_POINT ( 'NONE',  ( 10.19839929293505953, 1.581249999044084475, -24.62111388750000174 ) ) ;
#6092 = CARTESIAN_POINT ( 'NONE',  ( -17.40975659021753330, 4.018749999044084475, 17.40975659021752975 ) ) ;
#6093 = DIRECTION ( 'NONE',  ( 0.000000000000000000, -2.775557561562888270E-17, -1.000000000000000000 ) ) ;
#6094 = CARTESIAN_POINT ( 'NONE',  ( -24.62111388750000174, 4.656249999044085541, -10.19839929293506131 ) ) ;
#6095 = CARTESIAN_POINT ( 'NONE',  ( -17.40975659021752975, 1.768749999044084475, -17.40975659021752975 ) ) ;
#6096 = ORIENTED_EDGE ( 'NONE', *, *, #2086, .T. ) ;
#6097 = CARTESIAN_POINT ( 'NONE',  ( 13.63990010960492860, 25.00000000000000000, 7.874999999999965361 ) ) ;
#6098 =( NAMED_UNIT ( * ) SI_UNIT ( $, .STERADIAN. ) SOLID_ANGLE_UNIT ( ) );
#6099 = CARTESIAN_POINT ( 'NONE',  ( 1.530808498934191521E-15, 1.862499998088169129, -25.00000000000000000 ) ) ;
#6100 = FACE_OUTER_BOUND ( 'NONE', #8245, .T. ) ;
#6101 = CARTESIAN_POINT ( 'NONE',  ( -25.00000000000000000, 1.112499998088169351, -3.061616997868383043E-15 ) ) ;
#6102 = CARTESIAN_POINT ( 'NONE',  ( -13.63990010960481492, 25.00000000000000000, 7.875000000000163425 ) ) ;
#6103 = CARTESIAN_POINT ( 'NONE',  ( -25.00000000000000000, 3.437500000000000000, -10.35533905932738108 ) ) ;
#6104 = PRODUCT ( 'Central Drive Shaft', 'Central Drive Shaft', '', ( #1649 ) ) ;
#6105 = EDGE_LOOP ( 'NONE', ( #7706, #10866, #6000, #10603 ) ) ;
#6106 = CARTESIAN_POINT ( 'NONE',  ( 0.000000000000000000, 0.000000000000000000, 0.000000000000000000 ) ) ;
#6107 = CARTESIAN_POINT ( 'NONE',  ( -10.19839929293505776, 3.706249999044084920, -24.62111388750000174 ) ) ;
#6108 = CARTESIAN_POINT ( 'NONE',  ( 0.000000000000000000, 31.00000000000000000, 0.000000000000000000 ) ) ;
#6109 = CARTESIAN_POINT ( 'NONE',  ( 24.99999999999999289, 2.549999998088169129, 10.35533905932739529 ) ) ;
#6110 = CARTESIAN_POINT ( 'NONE',  ( -17.40975659021753330, 2.843749999044085097, 17.40975659021752975 ) ) ;
#6111 =( NAMED_UNIT ( * ) SI_UNIT ( $, .STERADIAN. ) SOLID_ANGLE_UNIT ( ) );
#6112 = CARTESIAN_POINT ( 'NONE',  ( 0.000000000000000000, 10.00000000000000355, 0.000000000000000000 ) ) ;
#6113 = CARTESIAN_POINT ( 'NONE',  ( 6.062177826491077504, 20.00000000000000355, -3.499999999999985345 ) ) ;
#6114 = PLANE ( 'NONE',  #2313 ) ;
#6115 = DIRECTION ( 'NONE',  ( 0.000000000000000000, -1.000000000000000000, 0.000000000000000000 ) ) ;
#6116 = DIRECTION ( 'NONE',  ( -0.9449111825230702699, -0.000000000000000000, 0.3273268353539822706 ) ) ;
#6117 = ORIENTED_EDGE ( 'NONE', *, *, #8473, .F. ) ;
#6118 = ORIENTED_EDGE ( 'NONE', *, *, #10232, .F. ) ;
#6119 = VERTEX_POINT ( 'NONE', #7680 ) ;
#6120 = VERTEX_POINT ( 'NONE', #9324 ) ;
#6121 = DIRECTION ( 'NONE',  ( 1.000000000000000000, 0.000000000000000000, 0.000000000000000000 ) ) ;
#6122 = DIRECTION ( 'NONE',  ( 0.4330127018922192428, -0.8660254037844380415, 0.2500000000000026645 ) ) ;
#6123 = CYLINDRICAL_SURFACE ( 'NONE', #4501, 2.999999999999997780 ) ;
#6124 = CARTESIAN_POINT ( 'NONE',  ( 3.050810944027392283E-15, -55.00000000000000000, -24.91176187412963117 ) ) ;
#6125 = CARTESIAN_POINT ( 'NONE',  ( 2.999999999999996447, 25.00000000000000000, -19.75000000000000000 ) ) ;
#6126 = EDGE_CURVE ( 'NONE', #6508, #10522, #5974, .T. ) ;
#6127 = CARTESIAN_POINT ( 'NONE',  ( 7.874999999999916511, 25.00000000000000000, -13.63990010960495702 ) ) ;
#6128 = FACE_OUTER_BOUND ( 'NONE', #7508, .T. ) ;
#6129 = DIRECTION ( 'NONE',  ( 0.000000000000000000, 1.000000000000000000, 0.000000000000000000 ) ) ;
#6130 = EDGE_CURVE ( 'NONE', #4742, #7447, #2422, .T. ) ;
#6131 = ORIENTED_EDGE ( 'NONE', *, *, #5870, .F. ) ;
#6132 = CARTESIAN_POINT ( 'NONE',  ( -1.500000000000000444, 88.00000000000001421, 1.499999999999999778 ) ) ;
#6133 = CARTESIAN_POINT ( 'NONE',  ( 17.40975659021752620, 3.268749999044084475, 17.40975659021753330 ) ) ;
#6134 = CARTESIAN_POINT ( 'NONE',  ( 0.000000000000000000, 0.000000000000000000, 0.000000000000000000 ) ) ;
#6135 = ITEM_DEFINED_TRANSFORMATION ( 'NONE', 'NONE', #8102,  #7040 ) ;
#6136 = CYLINDRICAL_SURFACE ( 'NONE', #5895, 2.999999999999999112 ) ;
#6137 = DIRECTION ( 'NONE',  ( 0.000000000000000000, 0.000000000000000000, 1.000000000000000000 ) ) ;
#6138 = ADVANCED_FACE ( 'NONE', ( #8442 ), #3414, .T. ) ;
#6139 = CARTESIAN_POINT ( 'NONE',  ( -15.60400172474251868, -0.001000000000001000089, 12.47307621135349720 ) ) ;
#6140 = EDGE_LOOP ( 'NONE', ( #9261, #3261, #7231 ) ) ;
#6141 = EDGE_CURVE ( 'NONE', #4450, #8432, #6032, .T. ) ;
#6142 = LINE ( 'NONE', #9509, #7958 ) ;
#6143 = AXIS2_PLACEMENT_3D ( 'NONE', #3761, #3647, #2906 ) ;
#6144 = CARTESIAN_POINT ( 'NONE',  ( -17.40975659021752975, 4.593749999044084653, -17.40975659021752975 ) ) ;
#6145 = CARTESIAN_POINT ( 'NONE',  ( -20.63749999999999929, -1.533495552763497570E-16, -5.525000000000006573 ) ) ;
#6146 = ORIENTED_EDGE ( 'NONE', *, *, #1867, .T. ) ;
#6147 = DIRECTION ( 'NONE',  ( 0.5000000000000103251, 0.000000000000000000, 0.8660254037844327124 ) ) ;
#6148 = CARTESIAN_POINT ( 'NONE',  ( 15.74999999999999289, -0.001000000000001000089, -3.000000000000055955 ) ) ;
#6149 = CIRCLE ( 'NONE', #7540, 5.750000000000006217 ) ;
#6150 = CARTESIAN_POINT ( 'NONE',  ( -13.63990010960498367, -0.001000000000001000089, -7.874999999999870326 ) ) ;
#6151 = CARTESIAN_POINT ( 'NONE',  ( 10.35533905932737930, 0.7999999980881692396, -25.00000000000000000 ) ) ;
#6152 = ORIENTED_EDGE ( 'NONE', *, *, #5873, .T. ) ;
#6153 = VECTOR ( 'NONE', #6189, 1000.000000000000114 ) ;
#6154 = EDGE_LOOP ( 'NONE', ( #4053, #6801 ) ) ;
#6155 = ADVANCED_FACE ( 'NONE', ( #8389 ), #8340, .F. ) ;
#6156 = CARTESIAN_POINT ( 'NONE',  ( -10.19839929293507552, 2.081249999044084475, 24.62111388749999463 ) ) ;
#6157 = ORIENTED_EDGE ( 'NONE', *, *, #9566, .T. ) ;
#6158 = VECTOR ( 'NONE', #1295, 1000.000000000000000 ) ;
#6159 = FACE_OUTER_BOUND ( 'NONE', #3871, .T. ) ;
#6160 = CARTESIAN_POINT ( 'NONE',  ( 24.62111388750000174, 5.393749999044085364, 0.000000000000000000 ) ) ;
#6161 = CARTESIAN_POINT ( 'NONE',  ( -0.1339745962155587111, 10.00000000000000355, -12.92820323027550700 ) ) ;
#6162 = CARTESIAN_POINT ( 'NONE',  ( -10.35533905932737575, 2.924999998088168685, -25.00000000000000000 ) ) ;
#6163 = CARTESIAN_POINT ( 'NONE',  ( -24.62111388750000174, 4.656249999044085541, -10.19839929293506131 ) ) ;
#6164 = DIRECTION ( 'NONE',  ( -0.000000000000000000, 1.000000000000000000, -0.000000000000000000 ) ) ;
#6165 = CARTESIAN_POINT ( 'NONE',  ( 3.208128317448934119, 19.34316356887880772, -6.223805082245734255 ) ) ;
#6166 = FACE_OUTER_BOUND ( 'NONE', #1844, .T. ) ;
#6167 = DIRECTION ( 'NONE',  ( 0.000000000000000000, 1.000000000000000000, -0.000000000000000000 ) ) ;
#6168 = DIRECTION ( 'NONE',  ( 0.000000000000000000, -1.000000000000000000, 0.000000000000000000 ) ) ;
#6169 = AXIS2_PLACEMENT_3D ( 'NONE', #3654, #238, #2756 ) ;
#6170 = CARTESIAN_POINT ( 'NONE',  ( -17.67766952966368876, 0.3750000000000000000, -17.67766952966369232 ) ) ;
#6171 = FACE_OUTER_BOUND ( 'NONE', #179, .T. ) ;
#6172 = ORIENTED_EDGE ( 'NONE', *, *, #9031, .T. ) ;
#6173 = EDGE_LOOP ( 'NONE', ( #8247, #1449, #5919, #3860 ) ) ;
#6174 = CARTESIAN_POINT ( 'NONE',  ( 1.400000000000001910, 0.000000000000000000, 0.000000000000000000 ) ) ;
#6175 = DIRECTION ( 'NONE',  ( 0.000000000000000000, 1.000000000000000000, 0.000000000000000000 ) ) ;
#6176 = CARTESIAN_POINT ( 'NONE',  ( 24.81055694375000087, 0.1093749995220422710, 0.000000000000000000 ) ) ;
#6177 = CARTESIAN_POINT ( 'NONE',  ( 0.000000000000000000, 20.00000000000000355, 0.000000000000000000 ) ) ;
#6178 = DIRECTION ( 'NONE',  ( 0.9819805060619657411, -0.000000000000000000, 0.1889822365046139596 ) ) ;
#6179 = CARTESIAN_POINT ( 'NONE',  ( 2.850480947161637246, 19.75000000000000711, 5.937177826491089050 ) ) ;
#6180 = CARTESIAN_POINT ( 'NONE',  ( 1.530808498934191521E-15, 1.862499998088169129, -25.00000000000000000 ) ) ;
#6181 = CARTESIAN_POINT ( 'NONE',  ( -24.62111388750000174, 4.831249999044084475, -10.19839929293506131 ) ) ;
#6182 = ORIENTED_EDGE ( 'NONE', *, *, #2535, .F. ) ;
#6183 = ORIENTED_EDGE ( 'NONE', *, *, #688, .T. ) ;
#6184 = VECTOR ( 'NONE', #2388, 1000.000000000000000 ) ;
#6185 = ORIENTED_EDGE ( 'NONE', *, *, #9748, .F. ) ;
#6186 = EDGE_CURVE ( 'NONE', #7276, #6230, #8314, .T. ) ;
#6187 = EDGE_CURVE ( 'NONE', #6215, #9231, #782, .T. ) ;
#6188 = CARTESIAN_POINT ( 'NONE',  ( 1.399999999999998579, 0.000000000000000000, 0.000000000000000000 ) ) ;
#6189 = DIRECTION ( 'NONE',  ( 0.2500000000000010547, -0.8660254037844380415, -0.4330127018922199089 ) ) ;
#6190 = CARTESIAN_POINT ( 'NONE',  ( -17.40975659021752975, 1.768749999044084475, -17.40975659021752975 ) ) ;
#6191 = ORIENTED_EDGE ( 'NONE', *, *, #5275, .F. ) ;
#6192 = DIRECTION ( 'NONE',  ( -0.000000000000000000, 1.000000000000000000, -0.000000000000000000 ) ) ;
#6193 = CARTESIAN_POINT ( 'NONE',  ( 13.63990010960487353, 25.00000000000000000, -7.875000000000067502 ) ) ;
#6194 = VECTOR ( 'NONE', #3811, 1000.000000000000000 ) ;
#6195 = CIRCLE ( 'NONE', #1406, 2.999999999999999112 ) ;
#6196 = CARTESIAN_POINT ( 'NONE',  ( 0.000000000000000000, 10.00000000000000355, 0.000000000000000000 ) ) ;
#6197 = ADVANCED_FACE ( 'NONE', ( #8501 ), #3352, .T. ) ;
#6198 = EDGE_LOOP ( 'NONE', ( #7750, #5520, #8635 ) ) ;
#6199 = AXIS2_PLACEMENT_3D ( 'NONE', #4626, #7054, #5237 ) ;
#6200 = AXIS2_PLACEMENT_3D ( 'NONE', #937, #4305, #10930 ) ;
#6201 = EDGE_CURVE ( 'NONE', #5479, #2588, #9385, .T. ) ;
#6202 = ADVANCED_FACE ( 'NONE', ( #8559 ), #6749, .F. ) ;
#6203 = CARTESIAN_POINT ( 'NONE',  ( 0.000000000000000000, 7.000000000000003553, -4.500000000000000888 ) ) ;
#6204 = CARTESIAN_POINT ( 'NONE',  ( -20.63749999999999574, 1.126651916477732829E-15, 7.500000000000007994 ) ) ;
#6205 = CARTESIAN_POINT ( 'NONE',  ( -25.00000000000000000, 0.4374999999999999445, -10.35533905932738108 ) ) ;
#6206 = DIRECTION ( 'NONE',  ( -0.000000000000000000, -1.000000000000000000, -0.000000000000000000 ) ) ;
#6207 = DIRECTION ( 'NONE',  ( 0.000000000000000000, 0.000000000000000000, 1.000000000000000000 ) ) ;
#6208 = DIRECTION ( 'NONE',  ( 0.000000000000000000, 1.000000000000000000, 0.000000000000000000 ) ) ;
#6209 = CARTESIAN_POINT ( 'NONE',  ( -24.62111388750000174, 1.656249999044084431, -10.19839929293506131 ) ) ;
#6210 = DIRECTION ( 'NONE',  ( 0.000000000000000000, 1.000000000000000000, 0.000000000000000000 ) ) ;
#6211 = EDGE_CURVE ( 'NONE', #1446, #4908, #3293, .T. ) ;
#6212 = VECTOR ( 'NONE', #1855, 1000.000000000000000 ) ;
#6213 = AXIS2_PLACEMENT_3D ( 'NONE', #9022, #8295, #736 ) ;
#6214 = ORIENTED_EDGE ( 'NONE', *, *, #10430, .T. ) ;
#6215 = VERTEX_POINT ( 'NONE', #955 ) ;
#6216 = EDGE_CURVE ( 'NONE', #8398, #9751, #10111, .T. ) ;
#6217 = CARTESIAN_POINT ( 'NONE',  ( 0.000000000000000000, -58.00000000000000000, 0.000000000000000000 ) ) ;
#6218 = CARTESIAN_POINT ( 'NONE',  ( -10.19839929293507552, 1.906249999044084431, 24.62111388749999463 ) ) ;
#6219 = CARTESIAN_POINT ( 'NONE',  ( -4.522825247065398226E-15, 4.143749999044084475, 24.62111388750000174 ) ) ;
#6220 = CARTESIAN_POINT ( 'NONE',  ( -17.67766952966369232, 2.237499998088169573, 17.67766952966368876 ) ) ;
#6221 = CARTESIAN_POINT ( 'NONE',  ( -17.67766952966368876, 1.375000000000000000, -17.67766952966369232 ) ) ;
#6222 =( NAMED_UNIT ( * ) PLANE_ANGLE_UNIT ( ) SI_UNIT ( $, .RADIAN. ) );
#6223 = CIRCLE ( 'NONE', #4458, 2.999999999999997335 ) ;
#6224 = CARTESIAN_POINT ( 'NONE',  ( 9.875000000000023093, 25.00000000000000000, 17.10400172474264835 ) ) ;
#6225 = CARTESIAN_POINT ( 'NONE',  ( -17.67766952966369232, 2.625000000000000000, 17.67766952966368876 ) ) ;
#6226 = CARTESIAN_POINT ( 'NONE',  ( 18.60400172474263414, -0.001000000000001000089, -7.276923788646775471 ) ) ;
#6227 = EDGE_CURVE ( 'NONE', #824, #8414, #9219, .T. ) ;
#6228 = CARTESIAN_POINT ( 'NONE',  ( 24.99999999999999289, 1.937500000000000000, 10.35533905932739529 ) ) ;
#6229 = CARTESIAN_POINT ( 'NONE',  ( -3.058047309049933382, 10.00000000000000355, -6.296693311223948264 ) ) ;
#6230 = VERTEX_POINT ( 'NONE', #10164 ) ;
#6231 = CIRCLE ( 'NONE', #4470, 2.999999999999996891 ) ;
#6232 = EDGE_LOOP ( 'NONE', ( #8688, #8760, #4451, #3715, #7194 ) ) ;
#6233 = DIRECTION ( 'NONE',  ( -0.000000000000000000, -1.000000000000000000, -0.000000000000000000 ) ) ;
#6234 = VECTOR ( 'NONE', #9768, 1000.000000000000000 ) ;
#6235 = DIRECTION ( 'NONE',  ( 0.000000000000000000, 1.000000000000000000, 0.000000000000000000 ) ) ;
#6236 = VERTEX_POINT ( 'NONE', #5152 ) ;
#6237 = CARTESIAN_POINT ( 'NONE',  ( -12.47307621135311351, 25.00000000000000000, 15.60400172474282599 ) ) ;
#6238 = AXIS2_PLACEMENT_3D ( 'NONE', #7429, #9304, #4133 ) ;
#6239 = CARTESIAN_POINT ( 'NONE',  ( -1.500000000000000444, 83.00000000000000000, -1.500000000000000222 ) ) ;
#6240 = AXIS2_PLACEMENT_3D ( 'NONE', #5077, #867, #4237 ) ;
#6241 = DIRECTION ( 'NONE',  ( 0.000000000000000000, 0.000000000000000000, 1.000000000000000000 ) ) ;
#6242 = DIRECTION ( 'NONE',  ( 0.000000000000000000, -0.000000000000000000, 1.000000000000000000 ) ) ;
#6243 = CARTESIAN_POINT ( 'NONE',  ( 13.47724133595215790, 7.781088913245551630, 0.5000000000000470735 ) ) ;
#6244 = CARTESIAN_POINT ( 'NONE',  ( -24.62111388750000174, 4.893749999044084475, -3.015216831376932151E-15 ) ) ;
#6245 = AXIS2_PLACEMENT_3D ( 'NONE', #2668, #6235, #10254 ) ;
#6246 = AXIS2_PLACEMENT_3D ( 'NONE', #9397, #6985, #5327 ) ;
#6247 = ORIENTED_EDGE ( 'NONE', *, *, #5130, .F. ) ;
#6248 = AXIS2_PLACEMENT_3D ( 'NONE', #4340, #8642, #7704 ) ;
#6249 = CARTESIAN_POINT ( 'NONE',  ( 24.62111388750000174, 2.393749999044084475, 0.000000000000000000 ) ) ;
#6250 = VECTOR ( 'NONE', #9328, 1000.000000000000227 ) ;
#6251 = CARTESIAN_POINT ( 'NONE',  ( 0.000000000000000000, 20.00000000000000355, 0.000000000000000000 ) ) ;
#6252 = CONICAL_SURFACE ( 'NONE', #9051, 20.00000000000000000, 0.3947911196997613281 ) ;
#6253 = CARTESIAN_POINT ( 'NONE',  ( -1.500000000000000444, 83.00000000000000000, 1.499999999999999778 ) ) ;
#6254 = CYLINDRICAL_SURFACE ( 'NONE', #5882, 6.999999999999997335 ) ;
#6255 = ORIENTED_EDGE ( 'NONE', *, *, #3696, .F. ) ;
#6256 = VECTOR ( 'NONE', #4698, 1000.000000000000000 ) ;
#6257 = CARTESIAN_POINT ( 'NONE',  ( 0.000000000000000000, 10.00000000000000355, 0.000000000000000000 ) ) ;
#6258 = CARTESIAN_POINT ( 'NONE',  ( -17.67766952966369232, 0.6250000000000000000, 17.67766952966368876 ) ) ;
#6259 = CARTESIAN_POINT ( 'NONE',  ( 24.62111388750000174, 0.3937499990440845310, 0.000000000000000000 ) ) ;
#6260 = ORIENTED_EDGE ( 'NONE', *, *, #9519, .F. ) ;
#6261 = LINE ( 'NONE', #8015, #5466 ) ;
#6262 =( LENGTH_UNIT ( ) NAMED_UNIT ( * ) SI_UNIT ( .MILLI., .METRE. ) );
#6263 = LINE ( 'NONE', #392, #3034 ) ;
#6264 = CARTESIAN_POINT ( 'NONE',  ( -10.19839929293505776, 3.531249999044084653, -24.62111388750000174 ) ) ;
#6265 = CARTESIAN_POINT ( 'NONE',  ( 10.35533905932737930, 2.799999998088169573, -25.00000000000000000 ) ) ;
#6266 = ADVANCED_FACE ( 'NONE', ( #5918 ), #5091, .F. ) ;
#6267 = ADVANCED_FACE ( 'NONE', ( #1177, #4607 ), #232, .T. ) ;
#6268 = EDGE_CURVE ( 'NONE', #5295, #3918, #339, .T. ) ;
#6269 = ORIENTED_EDGE ( 'NONE', *, *, #7200, .T. ) ;
#6270 = ORIENTED_EDGE ( 'NONE', *, *, #4733, .T. ) ;
#6271 = EDGE_CURVE ( 'NONE', #2551, #1630, #9362, .T. ) ;
#6272 = DIRECTION ( 'NONE',  ( 0.000000000000000000, 0.8660254037844385966, -0.4999999999999998890 ) ) ;
#6273 = CARTESIAN_POINT ( 'NONE',  ( 24.62111388749999463, 3.156249999044084653, 10.19839929293507730 ) ) ;
#6274 = CARTESIAN_POINT ( 'NONE',  ( -24.62111388750000174, 4.893749999044085364, -3.015216831376932151E-15 ) ) ;
#6275 = CARTESIAN_POINT ( 'NONE',  ( 25.00000000000000000, 3.000000000000000000, 0.000000000000000000 ) ) ;
#6276 =( LENGTH_UNIT ( ) NAMED_UNIT ( * ) SI_UNIT ( .MILLI., .METRE. ) );
#6277 = CARTESIAN_POINT ( 'NONE',  ( 0.000000000000000000, 5.000000000000000000, -25.00000000000000000 ) ) ;
#6278 = DIRECTION ( 'NONE',  ( 0.000000000000000000, 0.000000000000000000, -1.000000000000000000 ) ) ;
#6279 = DIRECTION ( 'NONE',  ( 0.000000000000000000, 0.000000000000000000, -1.000000000000000000 ) ) ;
#6280 = EDGE_CURVE ( 'NONE', #2862, #7767, #7912, .T. ) ;
#6281 = ORIENTED_EDGE ( 'NONE', *, *, #3587, .T. ) ;
#6282 = ORIENTED_EDGE ( 'NONE', *, *, #7446, .F. ) ;
#6283 = VERTEX_POINT ( 'NONE', #7799 ) ;
#6284 = PRODUCT ( 'socket set screw cone point_iso_ISO 4027 - M4 x 16-N', 'socket set screw cone point_iso_ISO 4027 - M4 x 16-N', '', ( #5033 ) ) ;
#6285 =( BOUNDED_CURVE ( )  B_SPLINE_CURVE ( 2, ( #4681, #8032, #8132, #10568, #2977, #8960, #6385, #9736, #2169 ),
 .UNSPECIFIED., .F., .F. ) 
 B_SPLINE_CURVE_WITH_KNOTS ( ( 3, 2, 2, 2, 3 ),
 ( 0.1500000000000000222, 0.1750000000000000167, 0.2000000000000000389, 0.2250000000000000333, 0.2500000000000000000 ),
 .UNSPECIFIED. ) 
 CURVE ( )  GEOMETRIC_REPRESENTATION_ITEM ( )  RATIONAL_B_SPLINE_CURVE ( ( 0.9999999999999998890, 0.9238795325112868495, 1.000000000000000000, 0.9238795325112867385, 1.000000000000000000, 0.9238795325112867385, 1.000000000000000000, 0.9238795325112867385, 1.000000000000000000 ) ) 
 REPRESENTATION_ITEM ( '' )  );
#6286 = LINE ( 'NONE', #2118, #8780 ) ;
#6287 = EDGE_CURVE ( 'NONE', #3376, #2611, #2861, .T. ) ;
#6288 = DIRECTION ( 'NONE',  ( 0.000000000000000000, 0.000000000000000000, 1.000000000000000000 ) ) ;
#6289 = CARTESIAN_POINT ( 'NONE',  ( 12.47307621135333200, 28.00000000000000000, 15.60400172474264835 ) ) ;
#6290 = CARTESIAN_POINT ( 'NONE',  ( 0.000000000000000000, 10.00000000000000355, 0.000000000000000000 ) ) ;
#6291 = CARTESIAN_POINT ( 'NONE',  ( 1.499999999999999556, 83.00000000000000000, -1.500000000000000222 ) ) ;
#6292 = DIRECTION ( 'NONE',  ( 0.000000000000000000, -1.000000000000000000, 2.775557561562888270E-17 ) ) ;
#6293 = VERTEX_POINT ( 'NONE', #7086 ) ;
#6294 = EDGE_CURVE ( 'NONE', #69, #3614, #9037, .T. ) ;
#6295 = ORIENTED_EDGE ( 'NONE', *, *, #2735, .F. ) ;
#6296 = CARTESIAN_POINT ( 'NONE',  ( 0.4330127018922207971, 0.000000000000000000, -0.2499999999999974465 ) ) ;
#6297 = LINE ( 'NONE', #2948, #8649 ) ;
#6298 = CARTESIAN_POINT ( 'NONE',  ( 5.276923788646596947, 28.00000000000000000, -15.13990010960494459 ) ) ;
#6299 = CARTESIAN_POINT ( 'NONE',  ( 0.000000000000000000, -8.528980942125402365, 0.000000000000000000 ) ) ;
#6300 = CARTESIAN_POINT ( 'NONE',  ( -17.10400172474254532, -0.001000000000001000089, 9.875000000000202505 ) ) ;
#6301 = ORIENTED_EDGE ( 'NONE', *, *, #9970, .F. ) ;
#6302 = DIRECTION ( 'NONE',  ( 2.168404344971010347E-16, 0.000000000000000000, 1.000000000000000000 ) ) ;
#6303 = FACE_OUTER_BOUND ( 'NONE', #10836, .T. ) ;
#6304 = LINE ( 'NONE', #10446, #4279 ) ;
#6305 = EDGE_LOOP ( 'NONE', ( #2432, #1277, #9054, #4670, #5545 ) ) ;
#6306 = CARTESIAN_POINT ( 'NONE',  ( 1.530808498934191521E-15, 0.8624999980881691286, -25.00000000000000000 ) ) ;
#6307 = CARTESIAN_POINT ( 'NONE',  ( 2.632990618166809235E-16, 10.10000000000000497, 2.149999999999999911 ) ) ;
#6308 = COLOUR_RGB ( '', 0.66274510, 0.83137255, 0.94901961) ;
#6309 = CARTESIAN_POINT ( 'NONE',  ( 17.40975659021752975, 3.343749999044085097, -17.40975659021752975 ) ) ;
#6310 = CARTESIAN_POINT ( 'NONE',  ( 0.000000000000000000, 20.00000000000000355, 0.000000000000000000 ) ) ;
#6311 = ORIENTED_EDGE ( 'NONE', *, *, #9098, .F. ) ;
#6312 = EDGE_LOOP ( 'NONE', ( #7382, #6451, #7884, #7033, #9444, #977, #3009, #2116, #5616, #1745, #796, #8477, #1895, #10730, #2348, #10720, #7216 ) ) ;
#6313 = EDGE_LOOP ( 'NONE', ( #8660, #2152, #3332, #3065, #102, #3656 ) ) ;
#6314 = AXIS2_PLACEMENT_3D ( 'NONE', #9846, #2791, #8144 ) ;
#6315 = DIRECTION ( 'NONE',  ( 0.000000000000000000, 1.000000000000000000, 0.000000000000000000 ) ) ;
#6316 = CARTESIAN_POINT ( 'NONE',  ( -24.62111388750000174, 1.656249999044084431, -10.19839929293506131 ) ) ;
#6317 = VECTOR ( 'NONE', #2934, 1000.000000000000000 ) ;
#6318 = CARTESIAN_POINT ( 'NONE',  ( -10.19839929293505776, 3.706249999044084920, -24.62111388750000174 ) ) ;
#6319 = ORIENTED_EDGE ( 'NONE', *, *, #3645, .F. ) ;
#6320 = EDGE_CURVE ( 'NONE', #2942, #4797, #3593, .T. ) ;
#6321 = CARTESIAN_POINT ( 'NONE',  ( -25.00000000000001421, 4.562500000000000888, 10.35533905932737397 ) ) ;
#6322 =( NAMED_UNIT ( * ) PLANE_ANGLE_UNIT ( ) SI_UNIT ( $, .RADIAN. ) );
#6323 = CARTESIAN_POINT ( 'NONE',  ( 66.68467533811312364, 89.45240317130979690, -5.000000000000000000 ) ) ;
#6324 = DIRECTION ( 'NONE',  ( 1.000000000000000000, 0.000000000000000000, 0.000000000000000000 ) ) ;
#6325 = PLANE ( 'NONE',  #8674 ) ;
#6326 = CARTESIAN_POINT ( 'NONE',  ( 7.276923788646707969, -0.001000000000001000089, 18.60400172474265190 ) ) ;
#6327 =( GEOMETRIC_REPRESENTATION_CONTEXT ( 3 ) GLOBAL_UNCERTAINTY_ASSIGNED_CONTEXT ( ( #6707 ) ) GLOBAL_UNIT_ASSIGNED_CONTEXT ( ( #3665, #6222, #6111 ) ) REPRESENTATION_CONTEXT ( 'NONE', 'WORKASPACE' ) );
#6328 = EDGE_CURVE ( 'NONE', #4034, #8246, #6304, .T. ) ;
#6329 = VECTOR ( 'NONE', #3816, 1000.000000000000000 ) ;
#6330 = EDGE_LOOP ( 'NONE', ( #8706, #2589 ) ) ;
#6331 = ORIENTED_EDGE ( 'NONE', *, *, #4234, .T. ) ;
#6332 = ORIENTED_EDGE ( 'NONE', *, *, #5986, .T. ) ;
#6333 = EDGE_LOOP ( 'NONE', ( #8661, #8304, #305, #3565 ) ) ;
#6334 = CYLINDRICAL_SURFACE ( 'NONE', #9830, 2.149999999999999911 ) ;
#6335 = PRESENTATION_LAYER_ASSIGNMENT (  '', '', ( #8079 ) ) ;
#6336 = EDGE_CURVE ( 'NONE', #6450, #6764, #2699, .T. ) ;
#6337 = APPLICATION_CONTEXT ( 'automotive_design' ) ;
#6338 = AXIS2_PLACEMENT_3D ( 'NONE', #6991, #6, #10126 ) ;
#6339 = DIRECTION ( 'NONE',  ( 0.000000000000000000, 0.000000000000000000, 1.000000000000000000 ) ) ;
#6340 = LINE ( 'NONE', #6289, #5891 ) ;
#6341 = CARTESIAN_POINT ( 'NONE',  ( 11.26313972081439196, 10.00000000000000355, 6.348076211353378184 ) ) ;
#6342 = CARTESIAN_POINT ( 'NONE',  ( 13.63990010960487353, 28.00000000000000000, -7.875000000000067502 ) ) ;
#6343 = CARTESIAN_POINT ( 'NONE',  ( -10.35533905932737575, 3.312500000000000000, -25.00000000000000000 ) ) ;
#6344 = EDGE_CURVE ( 'NONE', #2046, #10543, #1945, .T. ) ;
#6345 =( BOUNDED_SURFACE ( )  B_SPLINE_SURFACE ( 1, 2, ( 
 ( #5989, #5169, #3545, #8517, #970, #2647, #4334, #7697, #4391, #7753, #6939, #10298, #6431, #10463, #4718, #3939, #7243, #2106, #3875, #7151, #5484, #3722, #456, #10614, #9731, #6377, #8797, #5593, #7193, #7974, #3779, #504, #406, #2161, #4768, #7100, #3031, #9781, #5544, #8123, #10672, #10515, #2058, #2213, #8748, #8904, #5435, #8953, #2971, #1339, #2920, #9580, #8848, #6318, #8071, #1383, #554, #9683, #7296, #1292, #6219, #4675, #2020, #5392, #10561, #3826, #1187, #4568, #2877, #4619, #1236, #7922, #6274, #8025, #350, #9631, #9066, #1661, #9882, #3183, #611 ),
 ( #8339, #6695, #5041, #2421, #8225, #4877, #9165, #2373, #7511, #4044, #832, #7562, #9831, #665, #10777, #7398, #781, #6583, #4826, #6476, #10834, #9942, #2317, #3992, #3083, #5802, #10051, #4151, #9218, #5748, #1599, #8182, #2264, #3234, #4985, #7457, #8388, #5648, #4099, #4200, #9006, #9110, #10890, #3292, #2472, #6633, #1545, #5860, #1432, #7344, #4929, #9991, #8277, #720, #10719, #3132, #5702, #6526, #1496, #1708, #9454, #1943, #6923, #10281, #2750, #3468, #2526, #3351, #2698, #4437, #6144, #6094, #9511, #1886, #7738, #8441, #231, #954, #5265, #5321, #1834 ) ),
 .UNSPECIFIED., .F., .F., .F. ) 
 B_SPLINE_SURFACE_WITH_KNOTS ( ( 2, 2 ),
 ( 3, 2, 2, 2, 2, 2, 2, 2, 2, 2, 2, 2, 2, 2, 2, 2, 2, 2, 2, 2, 2, 2, 2, 2, 2, 2, 2, 2, 2, 2, 2, 2, 2, 2, 2, 2, 2, 2, 2, 2, 3 ),
 ( 0.000000000000000000, 1.000000000000000000 ),
 ( 0.000000000000000000, 0.02500000000000000139, 0.05000000000000000278, 0.07499999999999999722, 0.1000000000000000056, 0.1250000000000000000, 0.1499999999999999944, 0.1749999999999999889, 0.2000000000000000111, 0.2250000000000000056, 0.2500000000000000000, 0.2750000000000000222, 0.2999999999999999889, 0.3250000000000000111, 0.3499999999999999778, 0.3750000000000000000, 0.4000000000000000222, 0.4249999999999999889, 0.4500000000000000111, 0.4749999999999999778, 0.5000000000000000000, 0.5250000000000000222, 0.5500000000000000444, 0.5749999999999999556, 0.5999999999999999778, 0.6250000000000000000, 0.6500000000000000222, 0.6750000000000000444, 0.6999999999999999556, 0.7249999999999999778, 0.7500000000000000000, 0.7750000000000000222, 0.8000000000000000444, 0.8249999999999999556, 0.8499999999999999778, 0.8750000000000000000, 0.9000000000000000222, 0.9250000000000000444, 0.9499999999999999556, 0.9749999999999999778, 1.000000000000000000 ),
 .UNSPECIFIED. ) 
 GEOMETRIC_REPRESENTATION_ITEM ( )  RATIONAL_B_SPLINE_SURFACE ( (
 ( 1.000000000000000000, 0.9238795325112867385, 1.000000000000000000, 0.9238795325112867385, 1.000000000000000000, 0.9238795325112867385, 1.000000000000000000, 0.9238795325112867385, 1.000000000000000000, 0.9238795325112867385, 1.000000000000000000, 0.9238795325112867385, 1.000000000000000000, 0.9238795325112867385, 1.000000000000000000, 0.9238795325112867385, 1.000000000000000000, 0.9238795325112867385, 1.000000000000000000, 0.9238795325112867385, 1.000000000000000000, 0.9238795325112867385, 1.000000000000000000, 0.9238795325112867385, 1.000000000000000000, 0.9238795325112867385, 1.000000000000000000, 0.9238795325112867385, 1.000000000000000000, 0.9238795325112867385, 1.000000000000000000, 0.9238795325112867385, 1.000000000000000000, 0.9238795325112867385, 1.000000000000000000, 0.9238795325112867385, 1.000000000000000000, 0.9238795325112867385, 1.000000000000000000, 0.9238795325112867385, 1.000000000000000000, 0.9238795325112867385, 1.000000000000000000, 0.9238795325112867385, 1.000000000000000000, 0.9238795325112867385, 1.000000000000000000, 0.9238795325112867385, 1.000000000000000000, 0.9238795325112867385, 1.000000000000000000, 0.9238795325112867385, 1.000000000000000000, 0.9238795325112867385, 1.000000000000000000, 0.9238795325112867385, 1.000000000000000000, 0.9238795325112867385, 1.000000000000000000, 0.9238795325112867385, 1.000000000000000000, 0.9238795325112867385, 1.000000000000000000, 0.9238795325112867385, 1.000000000000000000, 0.9238795325112867385, 1.000000000000000000, 0.9238795325112867385, 1.000000000000000000, 0.9238795325112867385, 1.000000000000000000, 0.9238795325112867385, 1.000000000000000000, 0.9238795325112867385, 1.000000000000000000, 0.9238795325112867385, 1.000000000000000000, 0.9238795325112867385, 1.000000000000000000, 0.9238795325112867385, 1.000000000000000000),
 ( 1.000000000000000000, 0.9238795325112867385, 1.000000000000000000, 0.9238795325112867385, 1.000000000000000000, 0.9238795325112867385, 1.000000000000000000, 0.9238795325112867385, 1.000000000000000000, 0.9238795325112867385, 1.000000000000000000, 0.9238795325112867385, 1.000000000000000000, 0.9238795325112867385, 1.000000000000000000, 0.9238795325112867385, 1.000000000000000000, 0.9238795325112867385, 1.000000000000000000, 0.9238795325112867385, 1.000000000000000000, 0.9238795325112867385, 1.000000000000000000, 0.9238795325112867385, 1.000000000000000000, 0.9238795325112867385, 1.000000000000000000, 0.9238795325112867385, 1.000000000000000000, 0.9238795325112867385, 1.000000000000000000, 0.9238795325112867385, 1.000000000000000000, 0.9238795325112867385, 1.000000000000000000, 0.9238795325112867385, 1.000000000000000000, 0.9238795325112867385, 1.000000000000000000, 0.9238795325112867385, 1.000000000000000000, 0.9238795325112867385, 1.000000000000000000, 0.9238795325112867385, 1.000000000000000000, 0.9238795325112867385, 1.000000000000000000, 0.9238795325112867385, 1.000000000000000000, 0.9238795325112867385, 1.000000000000000000, 0.9238795325112867385, 1.000000000000000000, 0.9238795325112867385, 1.000000000000000000, 0.9238795325112867385, 1.000000000000000000, 0.9238795325112867385, 1.000000000000000000, 0.9238795325112867385, 1.000000000000000000, 0.9238795325112867385, 1.000000000000000000, 0.9238795325112867385, 1.000000000000000000, 0.9238795325112867385, 1.000000000000000000, 0.9238795325112867385, 1.000000000000000000, 0.9238795325112867385, 1.000000000000000000, 0.9238795325112867385, 1.000000000000000000, 0.9238795325112867385, 1.000000000000000000, 0.9238795325112867385, 1.000000000000000000, 0.9238795325112867385, 1.000000000000000000, 0.9238795325112867385, 1.000000000000000000) ) ) 
 REPRESENTATION_ITEM ( '' )  SURFACE ( )  );
#6346 = ORIENTED_EDGE ( 'NONE', *, *, #6403, .T. ) ;
#6347 = FACE_OUTER_BOUND ( 'NONE', #4476, .T. ) ;
#6348 = DIRECTION ( 'NONE',  ( -1.000000000000000000, 0.000000000000000000, 1.047444401652940322E-14 ) ) ;
#6349 = CARTESIAN_POINT ( 'NONE',  ( -17.10400172474254532, 25.00000000000000000, 12.87500000000020250 ) ) ;
#6350 = EDGE_CURVE ( 'NONE', #2070, #10673, #3725, .T. ) ;
#6351 = DIRECTION ( 'NONE',  ( 0.000000000000000000, 0.000000000000000000, 1.000000000000000000 ) ) ;
#6352 = EDGE_CURVE ( 'NONE', #387, #5941, #8891, .T. ) ;
#6353 = PRODUCT_DEFINITION_FORMATION_WITH_SPECIFIED_SOURCE ( 'ANY', '', #451, .NOT_KNOWN. ) ;
#6354 = ORIENTED_EDGE ( 'NONE', *, *, #2748, .T. ) ;
#6355 = ORIENTED_EDGE ( 'NONE', *, *, #7132, .F. ) ;
#6356 = AXIS2_PLACEMENT_3D ( 'NONE', #6808, #10114, #892 ) ;
#6357 = DIRECTION ( 'NONE',  ( -0.000000000000000000, 1.000000000000000000, -0.000000000000000000 ) ) ;
#6358 = DIRECTION ( 'NONE',  ( 1.000000000000000000, 0.000000000000000000, -3.491481338843131383E-15 ) ) ;
#6359 = CARTESIAN_POINT ( 'NONE',  ( -21.06539724162749394, 5.000000000000003553, 12.88420918705474705 ) ) ;
#6360 = VECTOR ( 'NONE', #5049, 1000.000000000000114 ) ;
#6361 = CARTESIAN_POINT ( 'NONE',  ( 17.40975659021752620, 5.268749999044085364, 17.40975659021753330 ) ) ;
#6362 = ORIENTED_EDGE ( 'NONE', *, *, #8832, .F. ) ;
#6363 = DIRECTION ( 'NONE',  ( -0.5000000000000009992, -0.8660254037844380415, -5.237222008264710288E-15 ) ) ;
#6364 = SURFACE_SIDE_STYLE ('',( #3017 ) ) ;
#6365 = DIRECTION ( 'NONE',  ( -0.000000000000000000, 1.000000000000000000, -0.000000000000000000 ) ) ;
#6366 = EDGE_CURVE ( 'NONE', #4908, #3339, #9814, .T. ) ;
#6367 = CARTESIAN_POINT ( 'NONE',  ( -24.62111388750000884, 1.781249999044084875, 10.19839929293505421 ) ) ;
#6368 = CARTESIAN_POINT ( 'NONE',  ( 10.35533905932737930, 0.1874999999999999722, -25.00000000000000000 ) ) ;
#6369 = PRODUCT_DEFINITION_SHAPE ( 'NONE', 'NONE',  #8124 ) ;
#6370 = ORIENTED_EDGE ( 'NONE', *, *, #8806, .T. ) ;
#6371 = VECTOR ( 'NONE', #9929, 1000.000000000000000 ) ;
#6372 = ORIENTED_EDGE ( 'NONE', *, *, #585, .F. ) ;
#6373 = AXIS2_PLACEMENT_3D ( 'NONE', #8499, #10218, #108 ) ;
#6374 = ORIENTED_EDGE ( 'NONE', *, *, #9156, .F. ) ;
#6375 = LINE ( 'NONE', #7972, #5488 ) ;
#6376 = CARTESIAN_POINT ( 'NONE',  ( 10.19839929293505953, 1.406249999044084653, -24.62111388750000174 ) ) ;
#6377 = CARTESIAN_POINT ( 'NONE',  ( -24.62111388750000884, 1.956249999044084475, 10.19839929293505421 ) ) ;
#6378 = CARTESIAN_POINT ( 'NONE',  ( 17.67766952966369232, 2.125000000000000000, -17.67766952966369232 ) ) ;
#6379 =( NAMED_UNIT ( * ) PLANE_ANGLE_UNIT ( ) SI_UNIT ( $, .RADIAN. ) );
#6380 = AXIS2_PLACEMENT_3D ( 'NONE', #1137, #6315, #4617 ) ;
#6381 = VECTOR ( 'NONE', #4185, 1000.000000000000000 ) ;
#6382 = CARTESIAN_POINT ( 'NONE',  ( 13.63990010960487353, 25.00000000000000000, -4.875000000000069278 ) ) ;
#6383 = CARTESIAN_POINT ( 'NONE',  ( 10.35533905932737930, 1.799999998088168907, -25.00000000000000000 ) ) ;
#6384 = CYLINDRICAL_SURFACE ( 'NONE', #7806, 2.999999999999999112 ) ;
#6385 = CARTESIAN_POINT ( 'NONE',  ( 17.67766952966369232, 1.125000000000000222, -17.67766952966369232 ) ) ;
#6386 = ORIENTED_EDGE ( 'NONE', *, *, #8359, .T. ) ;
#6387 = ORIENTED_EDGE ( 'NONE', *, *, #3962, .T. ) ;
#6388 = ORIENTED_EDGE ( 'NONE', *, *, #478, .F. ) ;
#6389 = CARTESIAN_POINT ( 'NONE',  ( -4.592425496802574367E-15, 0.7500000000000000000, 25.00000000000000000 ) ) ;
#6390 = CIRCLE ( 'NONE', #10440, 4.500000000000000888 ) ;
#6391 = CARTESIAN_POINT ( 'NONE',  ( 1.530808498934191521E-15, 4.250000000000000000, -25.00000000000000000 ) ) ;
#6392 = LINE ( 'NONE', #5560, #2858 ) ;
#6393 = DIRECTION ( 'NONE',  ( -0.1889822365046077146, 0.000000000000000000, -0.9819805060619668513 ) ) ;
#6394 = DIRECTION ( 'NONE',  ( 0.5000000000000009992, 0.000000000000000000, -0.8660254037844380415 ) ) ;
#6395 = LINE ( 'NONE', #5563, #10287 ) ;
#6396 = AXIS2_PLACEMENT_3D ( 'NONE', #4049, #10001, #4882 ) ;
#6397 = EDGE_CURVE ( 'NONE', #2342, #3364, #3863, .T. ) ;
#6398 = ORIENTED_EDGE ( 'NONE', *, *, #10577, .T. ) ;
#6399 = ADVANCED_FACE ( 'NONE', ( #9980 ), #7500, .F. ) ;
#6400 = ORIENTED_EDGE ( 'NONE', *, *, #9778, .F. ) ;
#6401 = CIRCLE ( 'NONE', #3741, 12.77350269189627063 ) ;
#6402 = VERTEX_POINT ( 'NONE', #6677 ) ;
#6403 = EDGE_CURVE ( 'NONE', #7845, #8513, #6401, .T. ) ;
#6404 = CARTESIAN_POINT ( 'NONE',  ( 17.10400172474269098, 25.00000000000000000, 12.87499999999995559 ) ) ;
#6405 = DIRECTION ( 'NONE',  ( 0.000000000000000000, -1.000000000000000000, 0.000000000000000000 ) ) ;
#6406 = DIRECTION ( 'NONE',  ( -0.8660254037844433705, 0.000000000000000000, -0.4999999999999916733 ) ) ;
#6407 =( BOUNDED_CURVE ( )  B_SPLINE_CURVE ( 3, ( #4586, #7934, #6072, #8593 ),
 .UNSPECIFIED., .F., .F. ) 
 B_SPLINE_CURVE_WITH_KNOTS ( ( 4, 4 ),
 ( 3.927175151554401999, 3.998664601439922528 ),
 .UNSPECIFIED. ) 
 CURVE ( )  GEOMETRIC_REPRESENTATION_ITEM ( )  RATIONAL_B_SPLINE_CURVE ( ( 1.000000000000000000, 0.9995741502243209453, 0.9995741502243209453, 1.000000000000000000 ) ) 
 REPRESENTATION_ITEM ( '' )  );
#6408 = CARTESIAN_POINT ( 'NONE',  ( 0.000000000000000000, 83.00000000000000000, 0.000000000000000000 ) ) ;
#6409 = VECTOR ( 'NONE', #3324, 1000.000000000000000 ) ;
#6410 = AXIS2_PLACEMENT_3D ( 'NONE', #2194, #5571, #1266 ) ;
#6411 = EDGE_CURVE ( 'NONE', #6283, #7302, #1619, .T. ) ;
#6412 = VECTOR ( 'NONE', #297, 1000.000000000000000 ) ;
#6413 = ORIENTED_EDGE ( 'NONE', *, *, #9507, .F. ) ;
#6414 = CIRCLE ( 'NONE', #6935, 5.999999999999999112 ) ;
#6415 = ADVANCED_FACE ( 'NONE', ( #823 ), #3371, .T. ) ;
#6416 = DIRECTION ( 'NONE',  ( 0.000000000000000000, -0.8660254037844380415, 0.5000000000000009992 ) ) ;
#6417 = CARTESIAN_POINT ( 'NONE',  ( 8.499999999999998224, 92.59807621135333022, 5.000000000000000000 ) ) ;
#6418 = CARTESIAN_POINT ( 'NONE',  ( 6.062177826491077504, 20.00000000000000355, -3.499999999999985345 ) ) ;
#6419 = LINE ( 'NONE', #6466, #7287 ) ;
#6420 = VECTOR ( 'NONE', #4310, 1000.000000000000000 ) ;
#6421 = CARTESIAN_POINT ( 'NONE',  ( -17.40975659021753330, 2.843749999044085097, 17.40975659021752975 ) ) ;
#6422 = CARTESIAN_POINT ( 'NONE',  ( -5.276923788646812774, -0.001000000000001000089, -15.13990010960486821 ) ) ;
#6423 = VERTEX_POINT ( 'NONE', #2460 ) ;
#6424 = CIRCLE ( 'NONE', #7841, 5.525000000000006573 ) ;
#6425 = ORIENTED_EDGE ( 'NONE', *, *, #9514, .T. ) ;
#6426 = ORIENTED_EDGE ( 'NONE', *, *, #50, .T. ) ;
#6427 = ORIENTED_EDGE ( 'NONE', *, *, #5640, .T. ) ;
#6428 = AXIS2_PLACEMENT_3D ( 'NONE', #1475, #4858, #8203 ) ;
#6429 = CARTESIAN_POINT ( 'NONE',  ( -25.00000000000001421, 4.174999998088169129, 10.35533905932737397 ) ) ;
#6430 = CARTESIAN_POINT ( 'NONE',  ( 10.19839929293505953, 4.406249999044084653, -24.62111388750000174 ) ) ;
#6431 = CARTESIAN_POINT ( 'NONE',  ( -4.522825247065398226E-15, 1.143749999044084475, 24.62111388750000174 ) ) ;
#6432 = EDGE_LOOP ( 'NONE', ( #2964, #5876 ) ) ;
#6433 = CARTESIAN_POINT ( 'NONE',  ( -10.35533905932737575, 3.312500000000000000, -25.00000000000000000 ) ) ;
#6434 = LINE ( 'NONE', #10676, #7919 ) ;
#6435 = DIRECTION ( 'NONE',  ( -0.4330127018922226845, -0.8660254037844380415, 0.2499999999999965306 ) ) ;
#6436 = DIRECTION ( 'NONE',  ( 0.000000000000000000, 0.000000000000000000, 1.000000000000000000 ) ) ;
#6437 = CARTESIAN_POINT ( 'NONE',  ( 25.00000000000000000, 3.612499998088169129, 0.000000000000000000 ) ) ;
#6438 = VERTEX_POINT ( 'NONE', #5905 ) ;
#6439 = VERTEX_POINT ( 'NONE', #4971 ) ;
#6440 = CARTESIAN_POINT ( 'NONE',  ( 1.499999999999999556, 83.00000000000000000, -1.500000000000000222 ) ) ;
#6441 = FACE_OUTER_BOUND ( 'NONE', #2721, .T. ) ;
#6442 = DIRECTION ( 'NONE',  ( -0.8660254037844432595, 0.000000000000000000, 0.4999999999999919509 ) ) ;
#6443 = VERTEX_POINT ( 'NONE', #8321 ) ;
#6444 = DIRECTION ( 'NONE',  ( 0.000000000000000000, 0.000000000000000000, -1.000000000000000000 ) ) ;
#6445 = DIRECTION ( 'NONE',  ( -0.000000000000000000, 1.000000000000000000, -0.000000000000000000 ) ) ;
#6446 = CARTESIAN_POINT ( 'NONE',  ( 0.5000000000000000000, 0.000000000000000000, 0.000000000000000000 ) ) ;
#6447 = DIRECTION ( 'NONE',  ( 0.000000000000000000, 0.8660254037844380415, 0.5000000000000009992 ) ) ;
#6448 = VERTEX_POINT ( 'NONE', #5844 ) ;
#6449 = ORIENTED_EDGE ( 'NONE', *, *, #4093, .F. ) ;
#6450 = VERTEX_POINT ( 'NONE', #2513 ) ;
#6451 = ORIENTED_EDGE ( 'NONE', *, *, #2078, .T. ) ;
#6452 = CARTESIAN_POINT ( 'NONE',  ( -1.399999999999998579, 1.111629890924696344E-15, 7.400000000000007461 ) ) ;
#6453 = EDGE_CURVE ( 'NONE', #7963, #7140, #4913, .T. ) ;
#6454 = LINE ( 'NONE', #2235, #4842 ) ;
#6455 = CARTESIAN_POINT ( 'NONE',  ( 25.00000000000000000, 4.674999998088169129, -10.35533905932737753 ) ) ;
#6456 = FACE_OUTER_BOUND ( 'NONE', #4819, .T. ) ;
#6457 = LINE ( 'NONE', #2238, #1627 ) ;
#6458 = EDGE_CURVE ( 'NONE', #7784, #6293, #9574, .T. ) ;
#6459 = EDGE_LOOP ( 'NONE', ( #5789, #6473 ) ) ;
#6460 = LINE ( 'NONE', #9812, #1257 ) ;
#6461 = FILL_AREA_STYLE_COLOUR ( '', #1719 ) ;
#6462 = DIRECTION ( 'NONE',  ( 0.8660254037844382635, 0.5000000000000004441, 0.000000000000000000 ) ) ;
#6463 = VERTEX_POINT ( 'NONE', #9202 ) ;
#6464 = ADVANCED_FACE ( 'NONE', ( #1647 ), #5958, .F. ) ;
#6465 = LINE ( 'NONE', #3924, #4238 ) ;
#6466 = CARTESIAN_POINT ( 'NONE',  ( 3.050810944027392283E-15, -58.00000000000000000, -24.91176187412963117 ) ) ;
#6467 = ORIENTED_EDGE ( 'NONE', *, *, #1129, .F. ) ;
#6468 = LINE ( 'NONE', #9820, #7822 ) ;
#6469 = CARTESIAN_POINT ( 'NONE',  ( 24.62111388750000174, 1.218749999044084431, 0.000000000000000000 ) ) ;
#6470 = ORIENTED_EDGE ( 'NONE', *, *, #8400, .T. ) ;
#6471 = EDGE_CURVE ( 'NONE', #9481, #4659, #2326, .T. ) ;
#6472 = VERTEX_POINT ( 'NONE', #7552 ) ;
#6473 = ORIENTED_EDGE ( 'NONE', *, *, #5262, .T. ) ;
#6474 = CARTESIAN_POINT ( 'NONE',  ( -17.67766952966368876, 2.987499998088169129, -17.67766952966369232 ) ) ;
#6475 = LINE ( 'NONE', #1598, #3716 ) ;
#6476 = CARTESIAN_POINT ( 'NONE',  ( 10.19839929293505953, 1.406249999044084653, -24.62111388750000174 ) ) ;
#6477 = DIRECTION ( 'NONE',  ( 0.000000000000000000, 2.775557561562888270E-17, 1.000000000000000000 ) ) ;
#6478 = SURFACE_STYLE_USAGE ( .BOTH. , #10675 ) ;
#6479 = CARTESIAN_POINT ( 'NONE',  ( -6.994037468151967474, 19.34316356887880062, -0.3335819196119432228 ) ) ;
#6480 = LINE ( 'NONE', #2269, #2291 ) ;
#6481 = CARTESIAN_POINT ( 'NONE',  ( 0.000000000000000000, 28.00000000000000000, 0.000000000000000000 ) ) ;
#6482 = LINE ( 'NONE', #4725, #1977 ) ;
#6483 = EDGE_CURVE ( 'NONE', #7391, #1515, #984, .T. ) ;
#6484 = COLOUR_RGB ( '', 0.09019608, 0.27058824, 0.51372549) ;
#6485 = EDGE_LOOP ( 'NONE', ( #9572, #6718, #7501, #7768, #1286, #5117, #4060, #8963, #9790 ) ) ;
#6486 = ORIENTED_EDGE ( 'NONE', *, *, #5459, .T. ) ;
#6487 = AXIS2_PLACEMENT_3D ( 'NONE', #5607, #8967, #4783 ) ;
#6488 = DIRECTION ( 'NONE',  ( 0.000000000000000000, -2.775557561562888270E-17, -1.000000000000000000 ) ) ;
#6489 =( GEOMETRIC_REPRESENTATION_CONTEXT ( 3 ) GLOBAL_UNCERTAINTY_ASSIGNED_CONTEXT ( ( #9021 ) ) GLOBAL_UNIT_ASSIGNED_CONTEXT ( ( #10704, #10758, #10266 ) ) REPRESENTATION_CONTEXT ( 'NONE', 'WORKASPACE' ) );
#6490 = DIRECTION ( 'NONE',  ( 0.000000000000000000, 1.000000000000000000, 0.000000000000000000 ) ) ;
#6491 = CARTESIAN_POINT ( 'NONE',  ( -12.19615242270664979, 10.00000000000000355, 0.4999999999998722688 ) ) ;
#6492 = CIRCLE ( 'NONE', #8070, 2.999999999999997335 ) ;
#6493 = CARTESIAN_POINT ( 'NONE',  ( -17.40975659021752975, 2.593749999044084653, -17.40975659021752975 ) ) ;
#6494 = CYLINDRICAL_SURFACE ( 'NONE', #1634, 25.00000000000000000 ) ;
#6495 = ORIENTED_EDGE ( 'NONE', *, *, #4642, .T. ) ;
#6496 =( GEOMETRIC_REPRESENTATION_CONTEXT ( 3 ) GLOBAL_UNCERTAINTY_ASSIGNED_CONTEXT ( ( #10573 ) ) GLOBAL_UNIT_ASSIGNED_CONTEXT ( ( #4787, #571, #3095 ) ) REPRESENTATION_CONTEXT ( 'NONE', 'WORKASPACE' ) );
#6497 = ORIENTED_EDGE ( 'NONE', *, *, #5661, .T. ) ;
#6498 = ORIENTED_EDGE ( 'NONE', *, *, #6453, .T. ) ;
#6499 = VECTOR ( 'NONE', #3783, 999.9999999999998863 ) ;
#6500 = CYLINDRICAL_SURFACE ( 'NONE', #749, 6.750000000000007994 ) ;
#6501 = CARTESIAN_POINT ( 'NONE',  ( -3.924072712834500543, 19.03096903053431177, 5.796693311223878098 ) ) ;
#6502 = DIRECTION ( 'NONE',  ( 1.445602896647339163E-16, 0.000000000000000000, 1.000000000000000000 ) ) ;
#6503 = CARTESIAN_POINT ( 'NONE',  ( 13.63990010960492860, 28.00000000000000000, 7.874999999999965361 ) ) ;
#6504 = DIRECTION ( 'NONE',  ( 0.8660254037844402619, -0.4999999999999970579, 0.000000000000000000 ) ) ;
#6505 = AXIS2_PLACEMENT_3D ( 'NONE', #7626, #6930, #5222 ) ;
#6506 = ORIENTED_EDGE ( 'NONE', *, *, #4533, .F. ) ;
#6507 = EDGE_CURVE ( 'NONE', #5936, #3864, #5688, .T. ) ;
#6508 = VERTEX_POINT ( 'NONE', #4246 ) ;
#6509 = FILL_AREA_STYLE_COLOUR ( '', #4785 ) ;
#6510 = CARTESIAN_POINT ( 'NONE',  ( -17.40975659021753330, 3.018749999044084475, 17.40975659021752975 ) ) ;
#6511 = ORIENTED_EDGE ( 'NONE', *, *, #3464, .F. ) ;
#6512 = CARTESIAN_POINT ( 'NONE',  ( 3.673940397442059178E-15, 88.00000000000001421, 30.00000000000000000 ) ) ;
#6513 =( NAMED_UNIT ( * ) PLANE_ANGLE_UNIT ( ) SI_UNIT ( $, .RADIAN. ) );
#6514 = ADVANCED_FACE ( 'NONE', ( #38 ), #10208, .F. ) ;
#6515 = CARTESIAN_POINT ( 'NONE',  ( 1.530808498934191521E-15, 1.250000000000000000, -25.00000000000000000 ) ) ;
#6516 = CARTESIAN_POINT ( 'NONE',  ( -17.40975659021752975, 0.5937499990440846531, -17.40975659021752975 ) ) ;
#6517 = PRODUCT_DEFINITION_FORMATION_WITH_SPECIFIED_SOURCE ( 'ANY', '', #6104, .NOT_KNOWN. ) ;
#6518 = ORIENTED_EDGE ( 'NONE', *, *, #10713, .F. ) ;
#6519 = ORIENTED_EDGE ( 'NONE', *, *, #6530, .F. ) ;
#6520 = EDGE_CURVE ( 'NONE', #9493, #5323, #8933, .T. ) ;
#6521 = ADVANCED_FACE ( 'NONE', ( #3057 ), #1472, .F. ) ;
#6522 = VECTOR ( 'NONE', #493, 1000.000000000000000 ) ;
#6523 = CIRCLE ( 'NONE', #7941, 0.1000000000000002554 ) ;
#6524 = CARTESIAN_POINT ( 'NONE',  ( -17.67766952966368876, 3.987499998088168685, -17.67766952966369232 ) ) ;
#6525 = CARTESIAN_POINT ( 'NONE',  ( 5.276923788646599611, 25.00000000000000000, -15.13990010960494459 ) ) ;
#6526 = CARTESIAN_POINT ( 'NONE',  ( -24.62111388750000884, 3.781249999044084653, 10.19839929293505421 ) ) ;
#6527 = EDGE_LOOP ( 'NONE', ( #2091, #690, #5509, #4601, #9016, #1347, #8840, #5535, #8370, #2265, #7651, #4328, #633, #10681 ) ) ;
#6528 = DIRECTION ( 'NONE',  ( -1.000000000000000000, 0.000000000000000000, 0.000000000000000000 ) ) ;
#6529 = DIRECTION ( 'NONE',  ( 0.000000000000000000, 0.000000000000000000, 1.000000000000000000 ) ) ;
#6530 = EDGE_CURVE ( 'NONE', #6764, #6584, #2947, .T. ) ;
#6531 = CARTESIAN_POINT ( 'NONE',  ( 3.499999999999957812, 20.00000000000000355, 6.062177826491091714 ) ) ;
#6532 = LINE ( 'NONE', #2323, #697 ) ;
#6533 = CARTESIAN_POINT ( 'NONE',  ( 1.040834085586084257E-14, 90.00000000000001421, 0.000000000000000000 ) ) ;
#6534 = CARTESIAN_POINT ( 'NONE',  ( -1.399999999999998579, 0.000000000000000000, 0.000000000000000000 ) ) ;
#6535 = VECTOR ( 'NONE', #8338, 1000.000000000000114 ) ;
#6536 = ADVANCED_FACE ( 'NONE', ( #7267 ), #4643, .F. ) ;
#6537 = VERTEX_POINT ( 'NONE', #9655 ) ;
#6538 = VERTEX_POINT ( 'NONE', #8925 ) ;
#6539 = AXIS2_PLACEMENT_3D ( 'NONE', #454, #9524, #348 ) ;
#6540 = CIRCLE ( 'NONE', #4963, 6.750000000000007994 ) ;
#6541 = CARTESIAN_POINT ( 'NONE',  ( 1.507608415688466075E-15, 2.468749999044085097, -24.62111388750000174 ) ) ;
#6542 = DIRECTION ( 'NONE',  ( -0.4999999999999887312, 0.000000000000000000, 0.8660254037844451469 ) ) ;
#6543 = EDGE_CURVE ( 'NONE', #6537, #9241, #1410, .T. ) ;
#6544 = ORIENTED_EDGE ( 'NONE', *, *, #2029, .T. ) ;
#6545 = DIRECTION ( 'NONE',  ( 0.000000000000000000, 0.000000000000000000, 1.000000000000000000 ) ) ;
#6546 = CARTESIAN_POINT ( 'NONE',  ( 0.000000000000000000, 0.000000000000000000, 0.000000000000000000 ) ) ;
#6547 = CARTESIAN_POINT ( 'NONE',  ( -24.62111388750000174, 1.718749999044084431, -3.015216831376932151E-15 ) ) ;
#6548 = DIRECTION ( 'NONE',  ( 4.188538737677001009E-17, -0.9396926207859082059, 0.3420201433256694901 ) ) ;
#6549 = EDGE_LOOP ( 'NONE', ( #155, #2122, #7433, #9244 ) ) ;
#6550 = VECTOR ( 'NONE', #2958, 1000.000000000000000 ) ;
#6551 = ORIENTED_EDGE ( 'NONE', *, *, #6483, .F. ) ;
#6552 = AXIS2_PLACEMENT_3D ( 'NONE', #10305, #3668, #4525 ) ;
#6553 = ORIENTED_EDGE ( 'NONE', *, *, #4410, .T. ) ;
#6554 = DIRECTION ( 'NONE',  ( -0.000000000000000000, -1.000000000000000000, -0.000000000000000000 ) ) ;
#6555 = SHAPE_REPRESENTATION ( 'Inner Conical Burr Core', ( #7040 ), #1019 ) ;
#6556 = LINE ( 'NONE', #692, #10117 ) ;
#6557 = CARTESIAN_POINT ( 'NONE',  ( -6.999999999999997335, 20.00000000000000355, -6.917209860457518289E-14 ) ) ;
#6558 = AXIS2_PLACEMENT_3D ( 'NONE', #7155, #355, #5653 ) ;
#6559 = PLANE ( 'NONE',  #9924 ) ;
#6560 = FACE_OUTER_BOUND ( 'NONE', #901, .T. ) ;
#6561 = VECTOR ( 'NONE', #7513, 1000.000000000000000 ) ;
#6562 = ORIENTED_EDGE ( 'NONE', *, *, #8426, .T. ) ;
#6563 = AXIS2_PLACEMENT_3D ( 'NONE', #10169, #4263, #5419 ) ;
#6564 = FILL_AREA_STYLE ('',( #6509 ) ) ;
#6565 = CARTESIAN_POINT ( 'NONE',  ( -17.40975659021752975, 4.768749999044084475, -17.40975659021752975 ) ) ;
#6566 = VERTEX_POINT ( 'NONE', #8046 ) ;
#6567 = VECTOR ( 'NONE', #1517, 1000.000000000000000 ) ;
#6568 = CARTESIAN_POINT ( 'NONE',  ( 7.347880794884118750E-16, 28.00000000000000000, 5.999999999999999112 ) ) ;
#6569 = DIRECTION ( 'NONE',  ( 0.000000000000000000, 0.000000000000000000, 1.000000000000000000 ) ) ;
#6570 = FACE_BOUND ( 'NONE', #1222, .T. ) ;
#6571 = DIRECTION ( 'NONE',  ( 0.000000000000000000, 0.000000000000000000, 1.000000000000000000 ) ) ;
#6572 = CARTESIAN_POINT ( 'NONE',  ( 10.19839929293506486, 2.031249999044084653, 24.62111388749999819 ) ) ;
#6573 = AXIS2_PLACEMENT_3D ( 'NONE', #1865, #1041, #4413 ) ;
#6574 = AXIS2_PLACEMENT_3D ( 'NONE', #4892, #1510, #3050 ) ;
#6575 = VERTEX_POINT ( 'NONE', #8156 ) ;
#6576 = VERTEX_POINT ( 'NONE', #6404 ) ;
#6577 = AXIS2_PLACEMENT_3D ( 'NONE', #3473, #4155, #8345 ) ;
#6578 = ORIENTED_EDGE ( 'NONE', *, *, #3320, .T. ) ;
#6579 = AXIS2_PLACEMENT_3D ( 'NONE', #6627, #2464, #6571 ) ;
#6580 = CARTESIAN_POINT ( 'NONE',  ( 10.35533905932738286, 4.424999998088169129, 24.99999999999999645 ) ) ;
#6581 = LINE ( 'NONE', #3082, #6535 ) ;
#6582 = VECTOR ( 'NONE', #1031, 999.9999999999998863 ) ;
#6583 = CARTESIAN_POINT ( 'NONE',  ( 24.62111388750000174, 1.281249999044084653, -10.19839929293505776 ) ) ;
#6584 = VERTEX_POINT ( 'NONE', #9756 ) ;
#6585 = FACE_OUTER_BOUND ( 'NONE', #6016, .T. ) ;
#6586 =( NAMED_UNIT ( * ) SI_UNIT ( $, .STERADIAN. ) SOLID_ANGLE_UNIT ( ) );
#6587 = DIRECTION ( 'NONE',  ( 0.000000000000000000, 0.000000000000000000, 1.000000000000000000 ) ) ;
#6588 = EDGE_CURVE ( 'NONE', #7276, #9464, #6043, .T. ) ;
#6589 = CARTESIAN_POINT ( 'NONE',  ( 19.75000000000001066, 28.00000000000000000, 2.999999999999927613 ) ) ;
#6590 = AXIS2_PLACEMENT_3D ( 'NONE', #10480, #3681, #4412 ) ;
#6591 = DIRECTION ( 'NONE',  ( 0.000000000000000000, 0.000000000000000000, 1.000000000000000000 ) ) ;
#6592 = CARTESIAN_POINT ( 'NONE',  ( -13.47724133595216678, 7.781088913245558736, -0.5000000000001412204 ) ) ;
#6593 = AXIS2_PLACEMENT_3D ( 'NONE', #9369, #6787, #8423 ) ;
#6594 = DIRECTION ( 'NONE',  ( 0.9659258262890684232, -0.2588190451025202399, 0.000000000000000000 ) ) ;
#6595 = ORIENTED_EDGE ( 'NONE', *, *, #9720, .T. ) ;
#6596 = VERTEX_POINT ( 'NONE', #1361 ) ;
#6597 = EDGE_LOOP ( 'NONE', ( #4914, #5277, #8207, #10311 ) ) ;
#6598 = ADVANCED_FACE ( 'NONE', ( #3103 ), #5675, .T. ) ;
#6599 = EDGE_LOOP ( 'NONE', ( #4, #10022, #7655, #5659 ) ) ;
#6600 = DIRECTION ( 'NONE',  ( 0.000000000000000000, 0.000000000000000000, 1.000000000000000000 ) ) ;
#6601 = CARTESIAN_POINT ( 'NONE',  ( 6.296693311223896750, 10.00000000000000355, 3.058047309050043960 ) ) ;
#6602 = EDGE_CURVE ( 'NONE', #5770, #7097, #2082, .T. ) ;
#6603 = DIRECTION ( 'NONE',  ( 0.000000000000000000, 0.000000000000000000, 1.000000000000000000 ) ) ;
#6604 = DIRECTION ( 'NONE',  ( 0.4999999999999951705, 0.000000000000000000, -0.8660254037844413721 ) ) ;
#6605 = CARTESIAN_POINT ( 'NONE',  ( 24.62111388749999463, 4.156249999044083765, 10.19839929293507730 ) ) ;
#6606 = FACE_OUTER_BOUND ( 'NONE', #6198, .T. ) ;
#6607 = EDGE_LOOP ( 'NONE', ( #9317, #1122, #7593, #5027 ) ) ;
#6608 = ORIENTED_EDGE ( 'NONE', *, *, #4644, .F. ) ;
#6609 = ORIENTED_EDGE ( 'NONE', *, *, #2573, .F. ) ;
#6610 = ADVANCED_FACE ( 'NONE', ( #6347 ), #6500, .F. ) ;
#6611 = EDGE_LOOP ( 'NONE', ( #2917, #7861, #9607, #2636 ) ) ;
#6612 = FACE_OUTER_BOUND ( 'NONE', #6703, .T. ) ;
#6613 = LINE ( 'NONE', #1518, #4304 ) ;
#6614 = DIRECTION ( 'NONE',  ( 0.000000000000000000, -1.000000000000000000, 0.000000000000000000 ) ) ;
#6615 = CARTESIAN_POINT ( 'NONE',  ( 25.00000000000000000, 4.000000000000000000, 0.000000000000000000 ) ) ;
#6616 = PLANE ( 'NONE',  #10276 ) ;
#6617 = EDGE_CURVE ( 'NONE', #5941, #9902, #9856, .T. ) ;
#6618 = ORIENTED_EDGE ( 'NONE', *, *, #7215, .T. ) ;
#6619 = SURFACE_STYLE_USAGE ( .BOTH. , #3222 ) ;
#6620 = CARTESIAN_POINT ( 'NONE',  ( -7.875000000000116351, 28.00000000000000000, -13.63990010960484334 ) ) ;
#6621 = CARTESIAN_POINT ( 'NONE',  ( -24.62111388750000884, 0.9562499990440846975, 10.19839929293505421 ) ) ;
#6622 = ORIENTED_EDGE ( 'NONE', *, *, #1609, .F. ) ;
#6623 = CARTESIAN_POINT ( 'NONE',  ( 82.32050807568876394, 102.2820323027551410, 0.000000000000000000 ) ) ;
#6624 = APPLICATION_PROTOCOL_DEFINITION ( 'draft international standard', 'automotive_design', 1998, #1587 ) ;
#6625 = CARTESIAN_POINT ( 'NONE',  ( 0.000000000000000000, 7.000000000000003553, 0.000000000000000000 ) ) ;
#6626 = ORIENTED_EDGE ( 'NONE', *, *, #9810, .F. ) ;
#6627 = CARTESIAN_POINT ( 'NONE',  ( 0.000000000000000000, 27.99999999999999645, 0.000000000000000000 ) ) ;
#6628 = CARTESIAN_POINT ( 'NONE',  ( -24.62111388750000174, 1.656249999044084431, -10.19839929293506131 ) ) ;
#6629 = ORIENTED_EDGE ( 'NONE', *, *, #8957, .T. ) ;
#6630 = ORIENTED_EDGE ( 'NONE', *, *, #2219, .F. ) ;
#6631 = CARTESIAN_POINT ( 'NONE',  ( 10.19839929293505953, 0.5812499990440844755, -24.62111388750000174 ) ) ;
#6632 = FACE_OUTER_BOUND ( 'NONE', #2273, .T. ) ;
#6633 = CARTESIAN_POINT ( 'NONE',  ( 10.19839929293506486, 3.031249999044084653, 24.62111388749999819 ) ) ;
#6634 = CARTESIAN_POINT ( 'NONE',  ( 18.60400172474268032, -0.001000000000001000089, 7.276923788646641356 ) ) ;
#6635 = ORIENTED_EDGE ( 'NONE', *, *, #2650, .T. ) ;
#6636 = DIRECTION ( 'NONE',  ( -1.000000000000000000, 0.000000000000000000, 0.000000000000000000 ) ) ;
#6637 =( LENGTH_UNIT ( ) NAMED_UNIT ( * ) SI_UNIT ( .MILLI., .METRE. ) );
#6638 = SURFACE_SIDE_STYLE ('',( #9945 ) ) ;
#6639 = FACE_OUTER_BOUND ( 'NONE', #3560, .T. ) ;
#6640 = DIRECTION ( 'NONE',  ( 0.000000000000000000, 1.000000000000000000, 0.000000000000000000 ) ) ;
#6641 = FACE_OUTER_BOUND ( 'NONE', #5527, .T. ) ;
#6642 = CARTESIAN_POINT ( 'NONE',  ( 28.09696521099633060, 102.8977774788672264, -5.000000000000000000 ) ) ;
#6643 = ORIENTED_EDGE ( 'NONE', *, *, #2543, .F. ) ;
#6644 = ORIENTED_EDGE ( 'NONE', *, *, #5065, .F. ) ;
#6645 = ORIENTED_EDGE ( 'NONE', *, *, #6744, .T. ) ;
#6646 = ADVANCED_FACE ( 'NONE', ( #2293 ), #9040, .F. ) ;
#6647 = EDGE_CURVE ( 'NONE', #5829, #5968, #9585, .T. ) ;
#6648 = CARTESIAN_POINT ( 'NONE',  ( -24.62111388750000884, 2.956249999044084475, 10.19839929293505421 ) ) ;
#6649 = CARTESIAN_POINT ( 'NONE',  ( 24.62111388750000174, 0.2812499990440845976, -10.19839929293505776 ) ) ;
#6650 = PLANE ( 'NONE',  #153 ) ;
#6651 = ORIENTED_EDGE ( 'NONE', *, *, #8484, .F. ) ;
#6652 = DIRECTION ( 'NONE',  ( -1.000000000000000000, 0.000000000000000000, 1.445602896647339163E-16 ) ) ;
#6653 = FACE_BOUND ( 'NONE', #6232, .T. ) ;
#6654 = EDGE_CURVE ( 'NONE', #856, #457, #1631, .T. ) ;
#6655 = CARTESIAN_POINT ( 'NONE',  ( 25.00000000000000000, 4.612499998088169129, 0.000000000000000000 ) ) ;
#6656 = PRESENTATION_LAYER_ASSIGNMENT (  '', '', ( #1360 ) ) ;
#6657 = CARTESIAN_POINT ( 'NONE',  ( 1.507608415688466075E-15, 0.4687499990440845421, -24.62111388750000174 ) ) ;
#6658 = DIRECTION ( 'NONE',  ( 0.000000000000000000, 0.000000000000000000, -1.000000000000000000 ) ) ;
#6659 = ORIENTED_EDGE ( 'NONE', *, *, #3800, .F. ) ;
#6660 = ORIENTED_EDGE ( 'NONE', *, *, #8877, .F. ) ;
#6661 = VERTEX_POINT ( 'NONE', #4016 ) ;
#6662 = EDGE_CURVE ( 'NONE', #9231, #3965, #7370, .T. ) ;
#6663 = ORIENTED_EDGE ( 'NONE', *, *, #2066, .T. ) ;
#6664 = AXIS2_PLACEMENT_3D ( 'NONE', #6620, #3068, #4809 ) ;
#6665 = VECTOR ( 'NONE', #2176, 1000.000000000000114 ) ;
#6666 = LINE ( 'NONE', #10744, #8696 ) ;
#6667 = CARTESIAN_POINT ( 'NONE',  ( 0.000000000000000000, 88.00000000000001421, 0.000000000000000000 ) ) ;
#6668 = ADVANCED_FACE ( 'NONE', ( #1262 ), #7999, .T. ) ;
#6669 = DIRECTION ( 'NONE',  ( 0.000000000000000000, 1.502202555303639631E-16, 1.000000000000000000 ) ) ;
#6670 = CARTESIAN_POINT ( 'NONE',  ( -18.60400172474257730, 25.00000000000000000, 7.276923788646904256 ) ) ;
#6671 = CARTESIAN_POINT ( 'NONE',  ( 5.592313892344211723, 5.000000000000000000, 23.99629895547188951 ) ) ;
#6672 =( GEOMETRIC_REPRESENTATION_CONTEXT ( 3 ) GLOBAL_UNCERTAINTY_ASSIGNED_CONTEXT ( ( #3365 ) ) GLOBAL_UNIT_ASSIGNED_CONTEXT ( ( #6276, #8074, #8799 ) ) REPRESENTATION_CONTEXT ( 'NONE', 'WORKASPACE' ) );
#6673 = CIRCLE ( 'NONE', #9842, 4.000000000000006217 ) ;
#6674 = EDGE_LOOP ( 'NONE', ( #1417, #6831, #2445, #9262 ) ) ;
#6675 = FACE_BOUND ( 'NONE', #7451, .T. ) ;
#6676 = DIRECTION ( 'NONE',  ( -0.000000000000000000, 1.000000000000000000, -0.000000000000000000 ) ) ;
#6677 = CARTESIAN_POINT ( 'NONE',  ( 25.00000000000000000, -2.710505431213761085E-17, 0.000000000000000000 ) ) ;
#6678 = ADVANCED_FACE ( 'NONE', ( #10536 ), #10080, .T. ) ;
#6679 = ORIENTED_EDGE ( 'NONE', *, *, #3573, .F. ) ;
#6680 = DIRECTION ( 'NONE',  ( 0.000000000000000000, 0.000000000000000000, -1.000000000000000000 ) ) ;
#6681 = SHAPE_DEFINITION_REPRESENTATION ( #9440, #1269 ) ;
#6682 =( REPRESENTATION_RELATIONSHIP ('NONE','NONE', #1269, #6555 ) REPRESENTATION_RELATIONSHIP_WITH_TRANSFORMATION ( #4363 )SHAPE_REPRESENTATION_RELATIONSHIP( ) );
#6683 = ADVANCED_FACE ( 'NONE', ( #6612 ), #9139, .T. ) ;
#6684 = CARTESIAN_POINT ( 'NONE',  ( 1.530808498934191521E-15, 4.250000000000000000, -25.00000000000000000 ) ) ;
#6685 = ORIENTED_EDGE ( 'NONE', *, *, #4714, .T. ) ;
#6686 = CIRCLE ( 'NONE', #860, 0.1000000000000002554 ) ;
#6687 = CARTESIAN_POINT ( 'NONE',  ( 1.530808498934191521E-15, 3.250000000000000444, -25.00000000000000000 ) ) ;
#6688 = CARTESIAN_POINT ( 'NONE',  ( -24.62111388750000884, 2.781249999044085097, 10.19839929293505421 ) ) ;
#6689 = ORIENTED_EDGE ( 'NONE', *, *, #10507, .T. ) ;
#6690 =( BOUNDED_CURVE ( )  B_SPLINE_CURVE ( 3, ( #2319, #2424, #5705, #9112 ),
 .UNSPECIFIED., .F., .F. ) 
 B_SPLINE_CURVE_WITH_KNOTS ( ( 4, 4 ),
 ( 3.927175151554402888, 3.998664601439924304 ),
 .UNSPECIFIED. ) 
 CURVE ( )  GEOMETRIC_REPRESENTATION_ITEM ( )  RATIONAL_B_SPLINE_CURVE ( ( 1.000000000000000000, 0.9995741502243209453, 0.9995741502243209453, 1.000000000000000000 ) ) 
 REPRESENTATION_ITEM ( '' )  );
#6691 = ORIENTED_EDGE ( 'NONE', *, *, #591, .T. ) ;
#6692 = CARTESIAN_POINT ( 'NONE',  ( 17.40975659021752620, 3.268749999044084475, 17.40975659021753330 ) ) ;
#6693 = ADVANCED_FACE ( 'NONE', ( #1569 ), #3158, .F. ) ;
#6694 = CARTESIAN_POINT ( 'NONE',  ( 7.874999999999916511, 25.00000000000000000, -13.63990010960495702 ) ) ;
#6695 = CARTESIAN_POINT ( 'NONE',  ( 24.62111388750000174, 0.2812499990440845976, -10.19839929293505776 ) ) ;
#6696 = CARTESIAN_POINT ( 'NONE',  ( 2.500000000000000444, -1.000000000000003331, 0.5773502691896272854 ) ) ;
#6697 = ORIENTED_EDGE ( 'NONE', *, *, #5257, .F. ) ;
#6698 = CARTESIAN_POINT ( 'NONE',  ( 1.499999999999999556, 83.00000000000000000, -1.500000000000000222 ) ) ;
#6699 = CARTESIAN_POINT ( 'NONE',  ( 17.67766952966368521, 1.487499998088169129, 17.67766952966369232 ) ) ;
#6700 = DIRECTION ( 'NONE',  ( 0.000000000000000000, 1.000000000000000000, -0.000000000000000000 ) ) ;
#6701 = DIRECTION ( 'NONE',  ( -0.2499999999999950318, -0.8660254037844380415, -0.4330127018922234061 ) ) ;
#6702 = LINE ( 'NONE', #5098, #3322 ) ;
#6703 = EDGE_LOOP ( 'NONE', ( #2416, #4551, #1560, #9060 ) ) ;
#6704 = ORIENTED_EDGE ( 'NONE', *, *, #2033, .F. ) ;
#6705 = ORIENTED_EDGE ( 'NONE', *, *, #7210, .T. ) ;
#6706 = ORIENTED_EDGE ( 'NONE', *, *, #10172, .F. ) ;
#6707 = UNCERTAINTY_MEASURE_WITH_UNIT (LENGTH_MEASURE( 1.000000000000000082E-05 ), #3665, 'distance_accuracy_value', 'NONE');
#6708 = CARTESIAN_POINT ( 'NONE',  ( -4.522825247065398226E-15, 2.143749999044084920, 24.62111388750000174 ) ) ;
#6709 = LINE ( 'NONE', #2279, #10781 ) ;
#6710 = LINE ( 'NONE', #5005, #4027 ) ;
#6711 = VECTOR ( 'NONE', #4813, 1000.000000000000000 ) ;
#6712 = VECTOR ( 'NONE', #1733, 1000.000000000000227 ) ;
#6713 = CARTESIAN_POINT ( 'NONE',  ( -16.34320696848747190, 5.000000000000000888, 18.55420638975051517 ) ) ;
#6714 = DIRECTION ( 'NONE',  ( 0.000000000000000000, -1.000000000000000000, 0.000000000000000000 ) ) ;
#6715 = CARTESIAN_POINT ( 'NONE',  ( 10.19839929293506486, 1.031249999044084653, 24.62111388749999819 ) ) ;
#6716 = LINE ( 'NONE', #1797, #10810 ) ;
#6717 = ORIENTED_EDGE ( 'NONE', *, *, #641, .T. ) ;
#6718 = ORIENTED_EDGE ( 'NONE', *, *, #10848, .T. ) ;
#6719 = VECTOR ( 'NONE', #10258, 1000.000000000000000 ) ;
#6720 = AXIS2_PLACEMENT_3D ( 'NONE', #9941, #1431, #9164 ) ;
#6721 = ORIENTED_EDGE ( 'NONE', *, *, #7524, .F. ) ;
#6722 = EDGE_CURVE ( 'NONE', #4407, #631, #1453, .T. ) ;
#6723 = DIRECTION ( 'NONE',  ( 0.000000000000000000, -1.000000000000000000, 0.000000000000000000 ) ) ;
#6724 = CARTESIAN_POINT ( 'NONE',  ( 2.999999999999999112, 28.00000000000000000, 19.75000000000000000 ) ) ;
#6725 = CARTESIAN_POINT ( 'NONE',  ( 1.285879139104720831E-15, 31.00000000000000000, 10.50000000000000000 ) ) ;
#6726 = CIRCLE ( 'NONE', #9008, 5.000000000000000000 ) ;
#6727 = AXIS2_PLACEMENT_3D ( 'NONE', #8486, #5903, #9252 ) ;
#6728 = DIRECTION ( 'NONE',  ( 0.000000000000000000, -0.000000000000000000, 1.000000000000000000 ) ) ;
#6729 = ADVANCED_FACE ( 'NONE', ( #862 ), #8308, .T. ) ;
#6730 = CARTESIAN_POINT ( 'NONE',  ( 16.80656569248275289, 5.000000000000001776, 18.21376690724898850 ) ) ;
#6731 = EDGE_CURVE ( 'NONE', #9293, #399, #401, .T. ) ;
#6732 = ADVANCED_FACE ( 'NONE', ( #8420 ), #691, .F. ) ;
#6733 = VERTEX_POINT ( 'NONE', #7427 ) ;
#6734 = CARTESIAN_POINT ( 'NONE',  ( 17.10400172474261637, 25.00000000000000000, -9.875000000000085265 ) ) ;
#6735 = VECTOR ( 'NONE', #8918, 1000.000000000000000 ) ;
#6736 = CARTESIAN_POINT ( 'NONE',  ( -0.3335819196118703922, 19.34316356887877220, 6.994037468151971026 ) ) ;
#6737 = ORIENTED_EDGE ( 'NONE', *, *, #106, .F. ) ;
#6738 = DIRECTION ( 'NONE',  ( 1.156482317317872514E-15, 0.000000000000000000, 1.000000000000000000 ) ) ;
#6739 = FACE_OUTER_BOUND ( 'NONE', #4543, .T. ) ;
#6740 = CARTESIAN_POINT ( 'NONE',  ( -25.00000000000000000, 5.112499998088170017, -3.061616997868383043E-15 ) ) ;
#6741 = EDGE_CURVE ( 'NONE', #9902, #6215, #7629, .T. ) ;
#6742 = EDGE_LOOP ( 'NONE', ( #1258, #7408, #4137, #6386 ) ) ;
#6743 = VECTOR ( 'NONE', #5097, 1000.000000000000000 ) ;
#6744 = EDGE_CURVE ( 'NONE', #5745, #2067, #9971, .T. ) ;
#6745 = VECTOR ( 'NONE', #9512, 1000.000000000000000 ) ;
#6746 = CARTESIAN_POINT ( 'NONE',  ( -24.62111388750000174, 2.893749999044084475, -3.015216831376932151E-15 ) ) ;
#6747 = CARTESIAN_POINT ( 'NONE',  ( 10.35533905932740240, 1.812500000000000222, 24.99999999999998224 ) ) ;
#6748 = CARTESIAN_POINT ( 'NONE',  ( -3.500000000000040412, 20.00000000000000355, 6.062177826491044641 ) ) ;
#6749 = CYLINDRICAL_SURFACE ( 'NONE', #1997, 2.999999999999997335 ) ;
#6750 = ORIENTED_EDGE ( 'NONE', *, *, #5870, .T. ) ;
#6751 = CARTESIAN_POINT ( 'NONE',  ( -25.00000000000001066, 1.174999998088169351, 10.35533905932737397 ) ) ;
#6752 = SURFACE_SIDE_STYLE ('',( #10054 ) ) ;
#6753 = AXIS2_PLACEMENT_3D ( 'NONE', #482, #3912, #10746 ) ;
#6754 = CARTESIAN_POINT ( 'NONE',  ( 2.500000000000000444, -6.505213034913026604E-16, -1.154700538379252794 ) ) ;
#6755 = CIRCLE ( 'NONE', #1448, 2.000000000000000000 ) ;
#6756 = CARTESIAN_POINT ( 'NONE',  ( 0.000000000000000000, 85.00000000000000000, 0.000000000000000000 ) ) ;
#6757 = FACE_BOUND ( 'NONE', #1629, .T. ) ;
#6758 = CARTESIAN_POINT ( 'NONE',  ( 1.530808498934191521E-15, 4.250000000000000000, -25.00000000000000000 ) ) ;
#6759 =( BOUNDED_CURVE ( )  B_SPLINE_CURVE ( 2, ( #211, #4482, #2733, #10259, #1162, #7937, #10424, #2841, #1923 ),
 .UNSPECIFIED., .F., .F. ) 
 B_SPLINE_CURVE_WITH_KNOTS ( ( 3, 2, 2, 2, 3 ),
 ( 0.2500000000000000000, 0.2750000000000000222, 0.3000000000000000444, 0.3250000000000000666, 0.3500000000000000333 ),
 .UNSPECIFIED. ) 
 CURVE ( )  GEOMETRIC_REPRESENTATION_ITEM ( )  RATIONAL_B_SPLINE_CURVE ( ( 1.000000000000000000, 0.9238795325112867385, 1.000000000000000000, 0.9238795325112867385, 1.000000000000000000, 0.9238795325112867385, 1.000000000000000000, 0.9238795325112865164, 1.000000000000000222 ) ) 
 REPRESENTATION_ITEM ( '' )  );
#6760 = AXIS2_PLACEMENT_3D ( 'NONE', #7595, #4130, #10140 ) ;
#6761 = VECTOR ( 'NONE', #4976, 1000.000000000000000 ) ;
#6762 = ORIENTED_EDGE ( 'NONE', *, *, #6868, .T. ) ;
#6763 = VERTEX_POINT ( 'NONE', #3214 ) ;
#6764 = VERTEX_POINT ( 'NONE', #2397 ) ;
#6765 = VERTEX_POINT ( 'NONE', #8251 ) ;
#6766 = CARTESIAN_POINT ( 'NONE',  ( 5.796693311223918066, 19.03096903053432598, -3.924072712834439702 ) ) ;
#6767 = CARTESIAN_POINT ( 'NONE',  ( -24.62111388750000174, 0.6562499990440846531, -10.19839929293506131 ) ) ;
#6768 = CARTESIAN_POINT ( 'NONE',  ( -4.522825247065398226E-15, 1.143749999044084475, 24.62111388750000174 ) ) ;
#6769 = CARTESIAN_POINT ( 'NONE',  ( 17.40975659021752975, 0.3437499990440845421, -17.40975659021752975 ) ) ;
#6770 = LINE ( 'NONE', #7579, #2775 ) ;
#6771 = AXIS2_PLACEMENT_3D ( 'NONE', #2503, #7716, #6962 ) ;
#6772 = EDGE_CURVE ( 'NONE', #4001, #7375, #2857, .T. ) ;
#6773 = ORIENTED_EDGE ( 'NONE', *, *, #1952, .T. ) ;
#6774 = CARTESIAN_POINT ( 'NONE',  ( 1.499999999999999556, 83.00000000000000000, -1.500000000000000222 ) ) ;
#6775 = CARTESIAN_POINT ( 'NONE',  ( 14.00000000000000533, 0.000000000000000000, 2.000000000000004441 ) ) ;
#6776 = AXIS2_PLACEMENT_3D ( 'NONE', #8214, #9057, #7385 ) ;
#6777 = CARTESIAN_POINT ( 'NONE',  ( 25.00000000000000000, -2.710505431213761085E-17, 0.000000000000000000 ) ) ;
#6778 = DIRECTION ( 'NONE',  ( 0.5000000000000009992, 0.000000000000000000, -0.8660254037844380415 ) ) ;
#6779 = ORIENTED_EDGE ( 'NONE', *, *, #533, .T. ) ;
#6780 = ORIENTED_EDGE ( 'NONE', *, *, #6320, .T. ) ;
#6781 = AXIS2_PLACEMENT_3D ( 'NONE', #10082, #2670, #3325 ) ;
#6782 = CARTESIAN_POINT ( 'NONE',  ( 12.13990010960493748, -0.001000000000001000089, 10.47307621135328759 ) ) ;
#6783 = VECTOR ( 'NONE', #7372, 1000.000000000000000 ) ;
#6784 = DIRECTION ( 'NONE',  ( 1.000000000000000000, 0.000000000000000000, 3.491481338843133355E-15 ) ) ;
#6785 = FACE_OUTER_BOUND ( 'NONE', #4209, .T. ) ;
#6786 = CARTESIAN_POINT ( 'NONE',  ( 2.694222958124177204E-15, -0.5289809421253948152, 22.00000000000000355 ) ) ;
#6787 = DIRECTION ( 'NONE',  ( 0.000000000000000000, 1.000000000000000000, 0.000000000000000000 ) ) ;
#6788 = CARTESIAN_POINT ( 'NONE',  ( 6.062177826491054411, 20.00000000000000355, 3.500000000000023981 ) ) ;
#6789 = ORIENTED_EDGE ( 'NONE', *, *, #9427, .F. ) ;
#6790 = ORIENTED_EDGE ( 'NONE', *, *, #3076, .T. ) ;
#6791 = EDGE_CURVE ( 'NONE', #9241, #257, #227, .T. ) ;
#6792 = DIRECTION ( 'NONE',  ( 0.8660254037844382635, 0.5000000000000004441, 0.000000000000000000 ) ) ;
#6793 = CARTESIAN_POINT ( 'NONE',  ( 0.000000000000000000, 20.00000000000000355, 0.000000000000000000 ) ) ;
#6794 = DIRECTION ( 'NONE',  ( 1.000000000000000000, 0.000000000000000000, 0.000000000000000000 ) ) ;
#6795 = ORIENTED_EDGE ( 'NONE', *, *, #2925, .T. ) ;
#6796 = FACE_OUTER_BOUND ( 'NONE', #7367, .T. ) ;
#6797 = CARTESIAN_POINT ( 'NONE',  ( 1.214306433183764808E-14, 10.00000000000000355, 12.77350269189627063 ) ) ;
#6798 = LINE ( 'NONE', #10155, #2002 ) ;
#6799 = CARTESIAN_POINT ( 'NONE',  ( -24.62111388750000884, 3.781249999044084653, 10.19839929293505421 ) ) ;
#6800 = EDGE_CURVE ( 'NONE', #10642, #3303, #6666, .T. ) ;
#6801 = ORIENTED_EDGE ( 'NONE', *, *, #10158, .T. ) ;
#6802 = EDGE_CURVE ( 'NONE', #9220, #857, #5174, .T. ) ;
#6803 = CARTESIAN_POINT ( 'NONE',  ( -10.19839929293505776, 2.706249999044084475, -24.62111388750000174 ) ) ;
#6804 = CARTESIAN_POINT ( 'NONE',  ( 0.000000000000000000, 2.210487472460972698E-16, 1.610000000000000320 ) ) ;
#6805 = DIRECTION ( 'NONE',  ( 0.000000000000000000, -2.775557561562888270E-17, -1.000000000000000000 ) ) ;
#6806 = DIRECTION ( 'NONE',  ( -1.000000000000000000, 0.000000000000000000, 0.000000000000000000 ) ) ;
#6807 = ORIENTED_EDGE ( 'NONE', *, *, #7474, .T. ) ;
#6808 = CARTESIAN_POINT ( 'NONE',  ( -7.875000000000116351, 25.00000000000000000, -13.63990010960484334 ) ) ;
#6809 = FACE_BOUND ( 'NONE', #9175, .T. ) ;
#6810 = CARTESIAN_POINT ( 'NONE',  ( 10.35533905932738286, 1.424999998088169129, 24.99999999999999645 ) ) ;
#6811 = DIRECTION ( 'NONE',  ( 0.5000000000000073275, -0.000000000000000000, 0.8660254037844343777 ) ) ;
#6812 = CARTESIAN_POINT ( 'NONE',  ( -1.399999999999998579, 0.000000000000000000, 0.000000000000000000 ) ) ;
#6813 = ADVANCED_FACE ( 'NONE', ( #9915 ), #5830, .F. ) ;
#6814 = ORIENTED_EDGE ( 'NONE', *, *, #2535, .T. ) ;
#6815 = ORIENTED_EDGE ( 'NONE', *, *, #9857, .T. ) ;
#6816 = ORIENTED_EDGE ( 'NONE', *, *, #6216, .F. ) ;
#6817 = UNCERTAINTY_MEASURE_WITH_UNIT (LENGTH_MEASURE( 1.000000000000000082E-05 ), #4912, 'distance_accuracy_value', 'NONE');
#6818 = CARTESIAN_POINT ( 'NONE',  ( -2.999999999999997335, -0.001000000000001000089, 15.75000000000000355 ) ) ;
#6819 = CARTESIAN_POINT ( 'NONE',  ( -24.62111388750000174, 3.831249999044084920, -10.19839929293506131 ) ) ;
#6820 = LINE ( 'NONE', #5230, #6412 ) ;
#6821 = CARTESIAN_POINT ( 'NONE',  ( 17.40975659021752975, 2.518749999044084475, -17.40975659021752975 ) ) ;
#6822 = CARTESIAN_POINT ( 'NONE',  ( 25.00000000000000000, 1.062500000000000222, -10.35533905932737753 ) ) ;
#6823 = FILL_AREA_STYLE_COLOUR ( '', #1540 ) ;
#6824 = EDGE_CURVE ( 'NONE', #978, #9763, #1635, .T. ) ;
#6825 = DIRECTION ( 'NONE',  ( 0.000000000000000000, 0.000000000000000000, -1.000000000000000000 ) ) ;
#6826 = LINE ( 'NONE', #4119, #10585 ) ;
#6827 = CARTESIAN_POINT ( 'NONE',  ( -10.35533905932739174, 2.687500000000000444, 24.99999999999999289 ) ) ;
#6828 = CARTESIAN_POINT ( 'NONE',  ( -25.00000000000001066, 3.174999998088169573, 10.35533905932737397 ) ) ;
#6829 = ORIENTED_EDGE ( 'NONE', *, *, #6731, .T. ) ;
#6830 = ORIENTED_EDGE ( 'NONE', *, *, #3399, .T. ) ;
#6831 = ORIENTED_EDGE ( 'NONE', *, *, #8022, .T. ) ;
#6832 = ORIENTED_EDGE ( 'NONE', *, *, #8009, .F. ) ;
#6833 = DIRECTION ( 'NONE',  ( -0.000000000000000000, -1.000000000000000000, -0.000000000000000000 ) ) ;
#6834 = CARTESIAN_POINT ( 'NONE',  ( 24.62111388750000174, 0.3062499990440845643, 0.000000000000000000 ) ) ;
#6835 = ORIENTED_EDGE ( 'NONE', *, *, #3700, .T. ) ;
#6836 = CARTESIAN_POINT ( 'NONE',  ( 0.000000000000000000, 88.00000000000001421, 0.000000000000000000 ) ) ;
#6837 = DIRECTION ( 'NONE',  ( -0.000000000000000000, 1.000000000000000000, -0.000000000000000000 ) ) ;
#6838 = PLANE ( 'NONE',  #7641 ) ;
#6839 = FACE_OUTER_BOUND ( 'NONE', #8673, .T. ) ;
#6840 = FACE_OUTER_BOUND ( 'NONE', #2369, .T. ) ;
#6841 = ORIENTED_EDGE ( 'NONE', *, *, #3837, .F. ) ;
#6842 = SURFACE_STYLE_FILL_AREA ( #4140 ) ;
#6843 = CARTESIAN_POINT ( 'NONE',  ( -4.592425496802574367E-15, 4.750000000000000000, 25.00000000000000000 ) ) ;
#6844 = CARTESIAN_POINT ( 'NONE',  ( -0.1668442477450398642, 19.66631150450990617, 6.999999999999997335 ) ) ;
#6845 = VERTEX_POINT ( 'NONE', #813 ) ;
#6846 = CARTESIAN_POINT ( 'NONE',  ( 0.000000000000000000, -55.00000000000000000, 0.000000000000000000 ) ) ;
#6847 = CONTEXT_DEPENDENT_SHAPE_REPRESENTATION ( #8427, #8646 ) ;
#6848 = LINE ( 'NONE', #4250, #1470 ) ;
#6849 = VECTOR ( 'NONE', #4753, 1000.000000000000000 ) ;
#6850 = FACE_OUTER_BOUND ( 'NONE', #1018, .T. ) ;
#6851 = CARTESIAN_POINT ( 'NONE',  ( 10.19839929293506486, 5.031249999044084653, 24.62111388749999819 ) ) ;
#6852 = B_SPLINE_CURVE_WITH_KNOTS ( 'NONE', 3,
 ( #4168, #5995, #1507, #2486, #3310, #1561, #10071, #6713, #4888, #5883 ),
 .UNSPECIFIED., .F., .F.,
 ( 4, 2, 2, 2, 4 ),
 ( 0.000000000000000000, 0.006815791626871553661, 0.01363158325374310732, 0.02044737488061466185, 0.02726316650748621465 ),
 .UNSPECIFIED. ) ;
#6853 = TOROIDAL_SURFACE ( 'NONE', #9506, 6.250000000000000000, 0.7500000000000000000 ) ;
#6854 = EDGE_CURVE ( 'NONE', #2965, #5862, #4900, .T. ) ;
#6855 = CIRCLE ( 'NONE', #9840, 6.999999999999997335 ) ;
#6856 = CARTESIAN_POINT ( 'NONE',  ( 17.40975659021752975, 0.5187499990440846975, -17.40975659021752975 ) ) ;
#6857 = CARTESIAN_POINT ( 'NONE',  ( 10.19839929293506486, 3.206249999044084031, 24.62111388749999819 ) ) ;
#6858 = LINE ( 'NONE', #4199, #4616 ) ;
#6859 = AXIS2_PLACEMENT_3D ( 'NONE', #9272, #2532, #3598 ) ;
#6860 = DIRECTION ( 'NONE',  ( 1.000000000000000000, 0.000000000000000000, 0.000000000000000000 ) ) ;
#6861 = ORIENTED_EDGE ( 'NONE', *, *, #10533, .T. ) ;
#6862 = DIRECTION ( 'NONE',  ( 1.000000000000000000, 0.000000000000000000, -1.069128445102650095E-14 ) ) ;
#6863 = CYLINDRICAL_SURFACE ( 'NONE', #10106, 7.500000000000007994 ) ;
#6864 = FACE_BOUND ( 'NONE', #3196, .T. ) ;
#6865 = CARTESIAN_POINT ( 'NONE',  ( 25.00000000000000000, 0.6749999980881690176, -10.35533905932737753 ) ) ;
#6866 = DIRECTION ( 'NONE',  ( 0.000000000000000000, 1.000000000000000000, 0.000000000000000000 ) ) ;
#6867 = CARTESIAN_POINT ( 'NONE',  ( -25.00000000000000000, 4.437500000000000888, -10.35533905932738108 ) ) ;
#6868 = EDGE_CURVE ( 'NONE', #1630, #10532, #7060, .T. ) ;
#6869 = ADVANCED_FACE ( 'NONE', ( #1862 ), #1038, .T. ) ;
#6870 = EDGE_CURVE ( 'NONE', #1394, #9698, #3192, .T. ) ;
#6871 = EDGE_LOOP ( 'NONE', ( #1615, #1753, #2328, #2517, #1173 ) ) ;
#6872 = EDGE_LOOP ( 'NONE', ( #966, #8923, #2257, #3480 ) ) ;
#6873 = ORIENTED_EDGE ( 'NONE', *, *, #10175, .F. ) ;
#6874 = ADVANCED_FACE ( 'NONE', ( #87 ), #9203, .T. ) ;
#6875 = DIRECTION ( 'NONE',  ( -0.2499999999999950318, -0.8660254037844380415, -0.4330127018922235171 ) ) ;
#6876 = CARTESIAN_POINT ( 'NONE',  ( -24.62111388750000884, 0.7812499990440845421, 10.19839929293505421 ) ) ;
#6877 = DIRECTION ( 'NONE',  ( 1.000000000000000000, 0.000000000000000000, 0.000000000000000000 ) ) ;
#6878 = CARTESIAN_POINT ( 'NONE',  ( -17.67766952966369232, 3.237499998088169573, 17.67766952966368876 ) ) ;
#6879 = CARTESIAN_POINT ( 'NONE',  ( 24.62111388749999463, 3.156249999044084653, 10.19839929293507730 ) ) ;
#6880 = CARTESIAN_POINT ( 'NONE',  ( -10.35533905932737575, 2.924999998088169129, -25.00000000000000000 ) ) ;
#6881 = DIRECTION ( 'NONE',  ( 0.000000000000000000, -0.000000000000000000, 1.000000000000000000 ) ) ;
#6882 = FACE_BOUND ( 'NONE', #3613, .T. ) ;
#6883 = DIRECTION ( 'NONE',  ( 0.000000000000000000, 0.000000000000000000, 1.000000000000000000 ) ) ;
#6884 = CARTESIAN_POINT ( 'NONE',  ( 17.67766952966368521, 4.875000000000000000, 17.67766952966369232 ) ) ;
#6885 = EDGE_CURVE ( 'NONE', #3364, #3253, #40, .T. ) ;
#6886 = CARTESIAN_POINT ( 'NONE',  ( 0.000000000000000000, 10.10000000000000497, -2.149999999999999911 ) ) ;
#6887 =( GEOMETRIC_REPRESENTATION_CONTEXT ( 3 ) GLOBAL_UNCERTAINTY_ASSIGNED_CONTEXT ( ( #1504 ) ) GLOBAL_UNIT_ASSIGNED_CONTEXT ( ( #9671, #4557, #2203 ) ) REPRESENTATION_CONTEXT ( 'NONE', 'WORKASPACE' ) );
#6888 = ORIENTED_EDGE ( 'NONE', *, *, #1592, .T. ) ;
#6889 = ORIENTED_EDGE ( 'NONE', *, *, #7416, .T. ) ;
#6890 = ORIENTED_EDGE ( 'NONE', *, *, #1657, .T. ) ;
#6891 = PRODUCT_DEFINITION_SHAPE ( 'NONE', 'NONE',  #5432 ) ;
#6892 = ORIENTED_EDGE ( 'NONE', *, *, #9952, .T. ) ;
#6893 = DIRECTION ( 'NONE',  ( 0.000000000000000000, 0.000000000000000000, 1.000000000000000000 ) ) ;
#6894 = EDGE_CURVE ( 'NONE', #4742, #4838, #311, .T. ) ;
#6895 = AXIS2_PLACEMENT_3D ( 'NONE', #7346, #5805, #6528 ) ;
#6896 = AXIS2_PLACEMENT_3D ( 'NONE', #850, #4061, #8463 ) ;
#6897 = CARTESIAN_POINT ( 'NONE',  ( 5.665063509461043978, 10.00000000000000355, 10.81217782649112102 ) ) ;
#6898 = EDGE_LOOP ( 'NONE', ( #4183, #3318, #8686, #271 ) ) ;
#6899 = DIRECTION ( 'NONE',  ( 0.000000000000000000, 0.000000000000000000, -1.000000000000000000 ) ) ;
#6900 = FACE_OUTER_BOUND ( 'NONE', #4885, .T. ) ;
#6901 = DIRECTION ( 'NONE',  ( 0.000000000000000000, -1.000000000000000000, 0.000000000000000000 ) ) ;
#6902 = DIRECTION ( 'NONE',  ( 0.000000000000000000, 0.000000000000000000, -1.000000000000000000 ) ) ;
#6903 = DIRECTION ( 'NONE',  ( -0.000000000000000000, -1.000000000000000000, -0.000000000000000000 ) ) ;
#6904 = CARTESIAN_POINT ( 'NONE',  ( -17.40975659021753330, 4.018749999044084475, 17.40975659021752975 ) ) ;
#6905 = AXIS2_PLACEMENT_3D ( 'NONE', #2515, #8380, #4189 ) ;
#6906 = CIRCLE ( 'NONE', #6373, 5.000000000000005329 ) ;
#6907 =( REPRESENTATION_RELATIONSHIP ('NONE','NONE', #1269, #7612 ) REPRESENTATION_RELATIONSHIP_WITH_TRANSFORMATION ( #2742 )SHAPE_REPRESENTATION_RELATIONSHIP( ) );
#6908 = ORIENTED_EDGE ( 'NONE', *, *, #6411, .F. ) ;
#6909 = CIRCLE ( 'NONE', #5827, 25.00000000000000000 ) ;
#6910 = DIRECTION ( 'NONE',  ( -1.000000000000000000, 0.000000000000000000, 0.000000000000000000 ) ) ;
#6911 = CARTESIAN_POINT ( 'NONE',  ( -10.35533905932741128, 4.924999998088170905, -24.99999999999996803 ) ) ;
#6912 = CARTESIAN_POINT ( 'NONE',  ( -25.00000000000000000, 4.049999998088169129, -10.35533905932738108 ) ) ;
#6913 = VECTOR ( 'NONE', #1874, 1000.000000000000000 ) ;
#6914 = CARTESIAN_POINT ( 'NONE',  ( -24.62111388750000174, 4.893749999044084475, -3.015216831376932151E-15 ) ) ;
#6915 = EDGE_LOOP ( 'NONE', ( #4153, #1359, #10624 ) ) ;
#6916 = DIRECTION ( 'NONE',  ( -0.000000000000000000, -1.000000000000000000, -0.000000000000000000 ) ) ;
#6917 = ITEM_DEFINED_TRANSFORMATION ( 'NONE', 'NONE', #3872,  #7040 ) ;
#6918 = CARTESIAN_POINT ( 'NONE',  ( 0.000000000000000000, 10.00000000000000355, 0.000000000000000000 ) ) ;
#6919 = CYLINDRICAL_SURFACE ( 'NONE', #10293, 6.999999999999997335 ) ;
#6920 = CARTESIAN_POINT ( 'NONE',  ( -24.62111388750000174, 4.656249999044085541, -10.19839929293506131 ) ) ;
#6921 = CARTESIAN_POINT ( 'NONE',  ( -17.40975659021753330, 3.018749999044084475, 17.40975659021752975 ) ) ;
#6922 = DIRECTION ( 'NONE',  ( -0.000000000000000000, 1.000000000000000000, -0.000000000000000000 ) ) ;
#6923 = CARTESIAN_POINT ( 'NONE',  ( 17.40975659021752620, 4.093749999044084653, 17.40975659021753330 ) ) ;
#6924 = PRODUCT_DEFINITION ( 'UNKNOWN', '', #6517, #8802 ) ;
#6925 = CARTESIAN_POINT ( 'NONE',  ( 1.507608415688466075E-15, 1.643749999044084475, -24.62111388750000174 ) ) ;
#6926 = EDGE_LOOP ( 'NONE', ( #5306, #4782, #7590, #1529 ) ) ;
#6927 = CARTESIAN_POINT ( 'NONE',  ( 3.234507963899495005E-15, -58.00000000000000000, 24.91176187412963117 ) ) ;
#6928 = CARTESIAN_POINT ( 'NONE',  ( 24.99999999999999289, 1.549999998088169129, 10.35533905932739529 ) ) ;
#6929 = DIRECTION ( 'NONE',  ( 0.2499999999999979461, -0.8660254037844380415, 0.4330127018922216853 ) ) ;
#6930 = DIRECTION ( 'NONE',  ( 0.2588190451025202399, 0.9659258262890684232, -0.000000000000000000 ) ) ;
#6931 = DIRECTION ( 'NONE',  ( 0.000000000000000000, 1.000000000000000000, -0.000000000000000000 ) ) ;
#6932 = CARTESIAN_POINT ( 'NONE',  ( 25.00000000000000000, 3.062500000000000000, -10.35533905932737753 ) ) ;
#6933 = AXIS2_PLACEMENT_3D ( 'NONE', #2064, #3728, #6436 ) ;
#6934 = VERTEX_POINT ( 'NONE', #6897 ) ;
#6935 = AXIS2_PLACEMENT_3D ( 'NONE', #4480, #1006, #3235 ) ;
#6936 = LINE ( 'NONE', #6818, #5291 ) ;
#6937 = CARTESIAN_POINT ( 'NONE',  ( 24.62111388750000174, 4.456249999044085364, -10.19839929293505776 ) ) ;
#6938 = VECTOR ( 'NONE', #6447, 1000.000000000000000 ) ;
#6939 = CARTESIAN_POINT ( 'NONE',  ( -17.40975659021753330, 1.018749999044084698, 17.40975659021752975 ) ) ;
#6940 = EDGE_CURVE ( 'NONE', #8379, #10642, #8161, .T. ) ;
#6941 = CARTESIAN_POINT ( 'NONE',  ( -25.00000000000001421, 2.174999998088169573, 10.35533905932737397 ) ) ;
#6942 = CARTESIAN_POINT ( 'NONE',  ( 24.62111388750000174, 3.218749999044084653, 0.000000000000000000 ) ) ;
#6943 = ADVANCED_FACE ( 'NONE', ( #262 ), #5407, .F. ) ;
#6944 = PLANE ( 'NONE',  #6552 ) ;
#6945 = AXIS2_PLACEMENT_3D ( 'NONE', #9745, #2389, #4006 ) ;
#6946 = CARTESIAN_POINT ( 'NONE',  ( -13.63990010960498367, 25.00000000000000000, -7.874999999999870326 ) ) ;
#6947 = CARTESIAN_POINT ( 'NONE',  ( -25.00000000000000000, 1.500000000000000000, -3.061616997868383043E-15 ) ) ;
#6948 = DIRECTION ( 'NONE',  ( -0.4999999999999888423, 0.000000000000000000, -0.8660254037844449249 ) ) ;
#6949 = EDGE_CURVE ( 'NONE', #2, #1843, #3621, .T. ) ;
#6950 = EDGE_LOOP ( 'NONE', ( #10094, #4893, #6750 ) ) ;
#6951 = VECTOR ( 'NONE', #185, 1000.000000000000000 ) ;
#6952 = ORIENTED_EDGE ( 'NONE', *, *, #9343, .T. ) ;
#6953 = EDGE_LOOP ( 'NONE', ( #1989, #4287, #3630, #2362 ) ) ;
#6954 = ORIENTED_EDGE ( 'NONE', *, *, #6397, .T. ) ;
#6955 = CIRCLE ( 'NONE', #10475, 5.000000000000000000 ) ;
#6956 = CIRCLE ( 'NONE', #7833, 4.999999999999987566 ) ;
#6957 = EDGE_CURVE ( 'NONE', #3898, #9950, #8714, .T. ) ;
#6958 = AXIS2_PLACEMENT_3D ( 'NONE', #3925, #655, #7285 ) ;
#6959 = DIRECTION ( 'NONE',  ( 0.000000000000000000, -2.775557561562887961E-17, -1.000000000000000000 ) ) ;
#6960 = CYLINDRICAL_SURFACE ( 'NONE', #5022, 30.00000000000000000 ) ;
#6961 = CARTESIAN_POINT ( 'NONE',  ( 0.000000000000000000, 10.00000000000000355, 0.000000000000000000 ) ) ;
#6962 = DIRECTION ( 'NONE',  ( 0.000000000000000000, 0.000000000000000000, -1.000000000000000000 ) ) ;
#6963 = DIRECTION ( 'NONE',  ( 0.5000000000000009992, 0.000000000000000000, 0.8660254037844380415 ) ) ;
#6964 = DIRECTION ( 'NONE',  ( -0.000000000000000000, -1.000000000000000000, -0.000000000000000000 ) ) ;
#6965 = CIRCLE ( 'NONE', #10820, 4.000000000000006217 ) ;
#6966 = ADVANCED_FACE ( 'NONE', ( #7008 ), #8535, .T. ) ;
#6967 = CARTESIAN_POINT ( 'NONE',  ( 10.19839929293505953, 3.581249999044085364, -24.62111388750000174 ) ) ;
#6968 = AXIS2_PLACEMENT_3D ( 'NONE', #221, #7905, #7947 ) ;
#6969 = ORIENTED_EDGE ( 'NONE', *, *, #10167, .F. ) ;
#6970 = VECTOR ( 'NONE', #8240, 1000.000000000000114 ) ;
#6971 = DIRECTION ( 'NONE',  ( 0.000000000000000000, 0.000000000000000000, 1.000000000000000000 ) ) ;
#6972 = CARTESIAN_POINT ( 'NONE',  ( -4.592425496802574367E-15, 4.362499998088169129, 25.00000000000000000 ) ) ;
#6973 = CARTESIAN_POINT ( 'NONE',  ( 17.40975659021752975, 2.518749999044084475, -17.40975659021752975 ) ) ;
#6974 = CARTESIAN_POINT ( 'NONE',  ( 0.000000000000000000, -8.000000000000000000, -27.91176187412962761 ) ) ;
#6975 = CARTESIAN_POINT ( 'NONE',  ( 9.875000000000023093, -0.001000000000001000089, 17.10400172474264835 ) ) ;
#6976 = EDGE_CURVE ( 'NONE', #2686, #3734, #4289, .T. ) ;
#6977 = CYLINDRICAL_SURFACE ( 'NONE', #4655, 6.999999999999997335 ) ;
#6978 = DIRECTION ( 'NONE',  ( -0.000000000000000000, -1.000000000000000000, -0.000000000000000000 ) ) ;
#6979 = CARTESIAN_POINT ( 'NONE',  ( -15.13990010960496235, 28.00000000000000000, -5.276923788646544544 ) ) ;
#6980 = DIRECTION ( 'NONE',  ( 0.000000000000000000, -2.775557561562888270E-17, -1.000000000000000000 ) ) ;
#6981 = CARTESIAN_POINT ( 'NONE',  ( 12.77350269189627063, 10.00000000000000355, 3.256982943917019352E-14 ) ) ;
#6982 = ORIENTED_EDGE ( 'NONE', *, *, #4994, .T. ) ;
#6983 = PLANE ( 'NONE',  #4603 ) ;
#6984 = CARTESIAN_POINT ( 'NONE',  ( -17.67766952966369232, 2.625000000000000000, 17.67766952966368876 ) ) ;
#6985 = DIRECTION ( 'NONE',  ( -1.069128445102650095E-14, 0.000000000000000000, -1.000000000000000000 ) ) ;
#6986 = CARTESIAN_POINT ( 'NONE',  ( 17.67766952966369232, 0.7374999980881691286, -17.67766952966369232 ) ) ;
#6987 = CARTESIAN_POINT ( 'NONE',  ( -17.67766952966368876, 3.375000000000000000, -17.67766952966369232 ) ) ;
#6988 = ORIENTED_EDGE ( 'NONE', *, *, #1512, .T. ) ;
#6989 = ORIENTED_EDGE ( 'NONE', *, *, #6328, .F. ) ;
#6990 = EDGE_CURVE ( 'NONE', #2070, #2069, #2727, .T. ) ;
#6991 = CARTESIAN_POINT ( 'NONE',  ( 0.000000000000000000, 31.00000000000000000, 0.000000000000000000 ) ) ;
#6992 = CARTESIAN_POINT ( 'NONE',  ( 10.19839929293506486, 3.206249999044084031, 24.62111388749999819 ) ) ;
#6993 = DIRECTION ( 'NONE',  ( -1.000000000000000000, 0.000000000000000000, 0.000000000000000000 ) ) ;
#6994 = CARTESIAN_POINT ( 'NONE',  ( -10.35533905932737575, 4.924999998088169129, -25.00000000000000000 ) ) ;
#6995 = CARTESIAN_POINT ( 'NONE',  ( 17.40975659021752620, 3.093749999044084653, 17.40975659021753330 ) ) ;
#6996 = DIRECTION ( 'NONE',  ( 0.000000000000000000, 1.000000000000000000, 0.000000000000000000 ) ) ;
#6997 = CARTESIAN_POINT ( 'NONE',  ( 13.63990010960487353, 28.00000000000000000, -4.875000000000069278 ) ) ;
#6998 = CARTESIAN_POINT ( 'NONE',  ( 0.5590169943749494497, 6.392864540189691546E-16, -6.750000000000007105 ) ) ;
#6999 = CARTESIAN_POINT ( 'NONE',  ( 0.000000000000000000, 85.00000000000000000, 0.000000000000000000 ) ) ;
#7000 = LINE ( 'NONE', #2828, #2498 ) ;
#7001 = ORIENTED_EDGE ( 'NONE', *, *, #9628, .T. ) ;
#7002 = EDGE_CURVE ( 'NONE', #8398, #4593, #9484, .T. ) ;
#7003 = EDGE_LOOP ( 'NONE', ( #5485, #7235 ) ) ;
#7004 = ADVANCED_FACE ( 'NONE', ( #9540 ), #5352, .F. ) ;
#7005 = VERTEX_POINT ( 'NONE', #9599 ) ;
#7006 = DIRECTION ( 'NONE',  ( -0.000000000000000000, -1.000000000000000000, -0.000000000000000000 ) ) ;
#7007 = EDGE_CURVE ( 'NONE', #2886, #2611, #2224, .T. ) ;
#7008 = FACE_OUTER_BOUND ( 'NONE', #3574, .T. ) ;
#7009 = DIRECTION ( 'NONE',  ( 0.000000000000000000, 1.000000000000000000, -0.000000000000000000 ) ) ;
#7010 = DIRECTION ( 'NONE',  ( -0.000000000000000000, 1.000000000000000000, -0.000000000000000000 ) ) ;
#7011 = CARTESIAN_POINT ( 'NONE',  ( 0.000000000000000000, 10.00000000000000355, 0.000000000000000000 ) ) ;
#7012 = CARTESIAN_POINT ( 'NONE',  ( 3.673940397442059178E-15, 85.00000000000000000, 30.00000000000000000 ) ) ;
#7013 = DIRECTION ( 'NONE',  ( -0.000000000000000000, -1.000000000000000000, -0.000000000000000000 ) ) ;
#7014 = EDGE_CURVE ( 'NONE', #3713, #9729, #409, .T. ) ;
#7015 = ORIENTED_EDGE ( 'NONE', *, *, #10438, .F. ) ;
#7016 = EDGE_CURVE ( 'NONE', #1515, #9174, #7639, .T. ) ;
#7017 = ORIENTED_EDGE ( 'NONE', *, *, #10575, .F. ) ;
#7018 = EDGE_CURVE ( 'NONE', #9241, #5226, #5186, .T. ) ;
#7019 = DIRECTION ( 'NONE',  ( -0.000000000000000000, 1.000000000000000000, -0.000000000000000000 ) ) ;
#7020 = DIRECTION ( 'NONE',  ( 1.000000000000000000, 0.000000000000000000, 3.491481338843133355E-15 ) ) ;
#7021 = CARTESIAN_POINT ( 'NONE',  ( 24.62111388749999108, 2.331249999044084475, 10.19839929293507730 ) ) ;
#7022 = ORIENTED_EDGE ( 'NONE', *, *, #7252, .F. ) ;
#7023 = CARTESIAN_POINT ( 'NONE',  ( 3.061616997868383043E-15, 85.00000000000000000, 25.00000000000000000 ) ) ;
#7024 = CYLINDRICAL_SURFACE ( 'NONE', #3375, 2.999999999999997335 ) ;
#7025 = CARTESIAN_POINT ( 'NONE',  ( 15.75000000000000000, 25.00000000000000000, -5.821397334365942453E-14 ) ) ;
#7026 =( GEOMETRIC_REPRESENTATION_CONTEXT ( 3 ) GLOBAL_UNCERTAINTY_ASSIGNED_CONTEXT ( ( #3953 ) ) GLOBAL_UNIT_ASSIGNED_CONTEXT ( ( #171, #9327, #113 ) ) REPRESENTATION_CONTEXT ( 'NONE', 'WORKASPACE' ) );
#7027 = ADVANCED_FACE ( 'NONE', ( #4933 ), #3897, .F. ) ;
#7028 = ADVANCED_FACE ( 'NONE', ( #7986 ), #48, .T. ) ;
#7029 = CARTESIAN_POINT ( 'NONE',  ( 3.058047309049978235, 10.00000000000000355, 6.296693311223928724 ) ) ;
#7030 = VECTOR ( 'NONE', #5917, 1000.000000000000000 ) ;
#7031 = CARTESIAN_POINT ( 'NONE',  ( -10.35533905932737575, 0.3125000000000000000, -25.00000000000000000 ) ) ;
#7032 = CARTESIAN_POINT ( 'NONE',  ( -17.40975659021753330, 1.018749999044084698, 17.40975659021752975 ) ) ;
#7033 = ORIENTED_EDGE ( 'NONE', *, *, #4156, .T. ) ;
#7034 = DIRECTION ( 'NONE',  ( -0.4999999999999919509, 0.000000000000000000, -0.8660254037844432595 ) ) ;
#7035 = CARTESIAN_POINT ( 'NONE',  ( -10.35533905932739174, 2.687500000000000444, 24.99999999999999289 ) ) ;
#7036 = VECTOR ( 'NONE', #3442, 1000.000000000000000 ) ;
#7037 = CARTESIAN_POINT ( 'NONE',  ( -10.19839929293507375, 0.9062499990440844311, 24.62111388749999108 ) ) ;
#7038 = CARTESIAN_POINT ( 'NONE',  ( -1.500000000000000444, 83.00000000000000000, 1.499999999999999778 ) ) ;
#7039 = EDGE_LOOP ( 'NONE', ( #10692, #4562, #465 ) ) ;
#7040 = AXIS2_PLACEMENT_3D ( 'NONE', #1904, #3431, #7048 ) ;
#7041 = VERTEX_POINT ( 'NONE', #7256 ) ;
#7042 = EDGE_CURVE ( 'NONE', #2806, #2292, #8710, .T. ) ;
#7043 = CIRCLE ( 'NONE', #8242, 25.00000000000000000 ) ;
#7044 = CARTESIAN_POINT ( 'NONE',  ( 17.40975659021752620, 4.093749999044084653, 17.40975659021753330 ) ) ;
#7045 = DIRECTION ( 'NONE',  ( 1.000000000000000000, 0.000000000000000000, -3.708321773340234242E-15 ) ) ;
#7046 = CARTESIAN_POINT ( 'NONE',  ( -25.00000000000000000, 3.049999998088169129, -10.35533905932738108 ) ) ;
#7047 = CARTESIAN_POINT ( 'NONE',  ( 24.99999999999999289, 4.937500000000001776, 10.35533905932739529 ) ) ;
#7048 = DIRECTION ( 'NONE',  ( 1.000000000000000000, 0.000000000000000000, 0.000000000000000000 ) ) ;
#7049 = PLANE ( 'NONE',  #2081 ) ;
#7050 = MANIFOLD_SOLID_BREP ( 'AdvancedHole1', #4380 ) ;
#7051 = PLANE ( 'NONE',  #4059 ) ;
#7052 = PRODUCT_DEFINITION_CONTEXT ( 'detailed design', #1046, 'design' ) ;
#7053 = CARTESIAN_POINT ( 'NONE',  ( -25.00000000000000000, 2.437500000000000444, -10.35533905932738108 ) ) ;
#7054 = DIRECTION ( 'NONE',  ( -0.000000000000000000, -1.000000000000000000, -0.000000000000000000 ) ) ;
#7055 = AXIS2_PLACEMENT_3D ( 'NONE', #3426, #7695, #2593 ) ;
#7056 = CARTESIAN_POINT ( 'NONE',  ( 0.2251666049839524120, 0.000000000000000000, 0.000000000000000000 ) ) ;
#7057 = ORIENTED_EDGE ( 'NONE', *, *, #2747, .T. ) ;
#7058 =( BOUNDED_CURVE ( )  B_SPLINE_CURVE ( 2, ( #1754, #7461, #1437, #8184, #7347, #8281, #4104, #10345, #61 ),
 .UNSPECIFIED., .F., .F. ) 
 B_SPLINE_CURVE_WITH_KNOTS ( ( 3, 2, 2, 2, 3 ),
 ( 0.2499999999999999722, 0.2750000000000000222, 0.2999999999999999889, 0.3250000000000000111, 0.3499999999999999778 ),
 .UNSPECIFIED. ) 
 CURVE ( )  GEOMETRIC_REPRESENTATION_ITEM ( )  RATIONAL_B_SPLINE_CURVE ( ( 1.000000000000000000, 0.9238795325112866275, 1.000000000000000000, 0.9238795325112867385, 1.000000000000000000, 0.9238795325112867385, 1.000000000000000000, 0.9238795325112867385, 1.000000000000000000 ) ) 
 REPRESENTATION_ITEM ( '' )  );
#7059 = PRODUCT_RELATED_PRODUCT_CATEGORY ( 'part', '', ( #4420 ) ) ;
#7060 = LINE ( 'NONE', #1155, #3025 ) ;
#7061 = PRODUCT_DEFINITION_FORMATION_WITH_SPECIFIED_SOURCE ( 'ANY', '', #4420, .NOT_KNOWN. ) ;
#7062 = CYLINDRICAL_SURFACE ( 'NONE', #1643, 5.000000000000000000 ) ;
#7063 = CARTESIAN_POINT ( 'NONE',  ( 0.000000000000000000, -58.00000000000000000, 0.000000000000000000 ) ) ;
#7064 = CARTESIAN_POINT ( 'NONE',  ( 8.660254037844401509, 90.00000000000001421, 5.000000000000000000 ) ) ;
#7065 = DIRECTION ( 'NONE',  ( 0.000000000000000000, 1.000000000000000000, 0.000000000000000000 ) ) ;
#7066 = DIRECTION ( 'NONE',  ( -3.469446951953616950E-15, 0.000000000000000000, 1.000000000000000000 ) ) ;
#7067 = DIRECTION ( 'NONE',  ( 0.8660254037844397068, 0.000000000000000000, -0.4999999999999979461 ) ) ;
#7068 = ORIENTED_EDGE ( 'NONE', *, *, #9694, .T. ) ;
#7069 = VECTOR ( 'NONE', #10341, 1000.000000000000000 ) ;
#7070 = VECTOR ( 'NONE', #7628, 1000.000000000000000 ) ;
#7071 = ORIENTED_EDGE ( 'NONE', *, *, #6949, .F. ) ;
#7072 = CARTESIAN_POINT ( 'NONE',  ( 24.62111388750000174, 5.393749999044085364, 0.000000000000000000 ) ) ;
#7073 = EDGE_CURVE ( 'NONE', #8063, #6443, #1352, .T. ) ;
#7074 = CARTESIAN_POINT ( 'NONE',  ( 10.19839929293505953, 3.581249999044085364, -24.62111388750000174 ) ) ;
#7075 = ADVANCED_FACE ( 'NONE', ( #5498 ), #10479, .F. ) ;
#7076 = DIRECTION ( 'NONE',  ( 0.000000000000000000, 1.000000000000000000, -0.000000000000000000 ) ) ;
#7077 = DIRECTION ( 'NONE',  ( -0.000000000000000000, -1.000000000000000000, -0.000000000000000000 ) ) ;
#7078 = AXIS2_PLACEMENT_3D ( 'NONE', #4248, #8606, #4425 ) ;
#7079 = AXIS2_PLACEMENT_3D ( 'NONE', #9686, #8130, #2110 ) ;
#7080 = CARTESIAN_POINT ( 'NONE',  ( 0.000000000000000000, 25.00000000000000000, 0.000000000000000000 ) ) ;
#7081 = ADVANCED_FACE ( 'NONE', ( #9169 ), #9646, .F. ) ;
#7082 = AXIS2_PLACEMENT_3D ( 'NONE', #6446, #10637, #3795 ) ;
#7083 = AXIS2_PLACEMENT_3D ( 'NONE', #2178, #5558, #2790 ) ;
#7084 = PLANE ( 'NONE',  #7581 ) ;
#7085 = DIRECTION ( 'NONE',  ( -0.000000000000000000, 1.000000000000000000, -0.000000000000000000 ) ) ;
#7086 = CARTESIAN_POINT ( 'NONE',  ( -12.77350269189627063, 10.00000000000000355, -1.344410693882025246E-13 ) ) ;
#7087 = ORIENTED_EDGE ( 'NONE', *, *, #459, .T. ) ;
#7088 = ADVANCED_FACE ( 'NONE', ( #2072, #8808 ), #3792, .F. ) ;
#7089 = CARTESIAN_POINT ( 'NONE',  ( -3.223142256880076948E-15, -0.001000000000001000089, -15.75000000000000000 ) ) ;
#7090 = CARTESIAN_POINT ( 'NONE',  ( 0.000000000000000000, 0.000000000000000000, 0.000000000000000000 ) ) ;
#7091 = DIRECTION ( 'NONE',  ( 0.000000000000000000, 0.000000000000000000, 1.000000000000000000 ) ) ;
#7092 = CARTESIAN_POINT ( 'NONE',  ( 24.62111388749999108, 1.156249999044084431, 10.19839929293507730 ) ) ;
#7093 = DIRECTION ( 'NONE',  ( 0.000000000000000000, -1.000000000000000000, 0.000000000000000000 ) ) ;
#7094 = AXIS2_PLACEMENT_3D ( 'NONE', #4322, #835, #2529 ) ;
#7095 = ORIENTED_EDGE ( 'NONE', *, *, #8287, .F. ) ;
#7096 = EDGE_CURVE ( 'NONE', #3067, #3039, #6955, .T. ) ;
#7097 = VERTEX_POINT ( 'NONE', #5046 ) ;
#7098 = LINE ( 'NONE', #295, #532 ) ;
#7099 = CARTESIAN_POINT ( 'NONE',  ( 24.62111388750000174, 2.281249999044085541, -10.19839929293505776 ) ) ;
#7100 = CARTESIAN_POINT ( 'NONE',  ( 10.19839929293505953, 2.581249999044084475, -24.62111388750000174 ) ) ;
#7101 = CARTESIAN_POINT ( 'NONE',  ( -10.35533905932739174, 1.687500000000000000, 24.99999999999999289 ) ) ;
#7102 = AXIS2_PLACEMENT_3D ( 'NONE', #2657, #3434, #1192 ) ;
#7103 = DIRECTION ( 'NONE',  ( 0.3273268353539987574, 0.000000000000000000, -0.9449111825230646078 ) ) ;
#7104 = CARTESIAN_POINT ( 'NONE',  ( -0.4330127018922207971, 0.000000000000000000, 0.2499999999999974465 ) ) ;
#7105 = CARTESIAN_POINT ( 'NONE',  ( 0.000000000000000000, 20.00000000000000355, 0.000000000000000000 ) ) ;
#7106 = EDGE_CURVE ( 'NONE', #8744, #6845, #948, .T. ) ;
#7107 = ORIENTED_EDGE ( 'NONE', *, *, #8080, .F. ) ;
#7108 = ORIENTED_EDGE ( 'NONE', *, *, #6824, .F. ) ;
#7109 = VECTOR ( 'NONE', #1841, 1000.000000000000000 ) ;
#7110 = ORIENTED_EDGE ( 'NONE', *, *, #10945, .T. ) ;
#7111 = DIRECTION ( 'NONE',  ( -1.224646799147353454E-16, 0.000000000000000000, -1.000000000000000000 ) ) ;
#7112 = AXIS2_PLACEMENT_3D ( 'NONE', #1699, #9254, #4142 ) ;
#7113 = DIRECTION ( 'NONE',  ( 0.4330127018922207971, -0.8660254037844380415, -0.2499999999999995282 ) ) ;
#7114 = CIRCLE ( 'NONE', #2329, 12.77350269189627063 ) ;
#7115 = CARTESIAN_POINT ( 'NONE',  ( -0.2499999999999990286, 0.000000000000000000, -0.4330127018922199644 ) ) ;
#7116 = AXIS2_PLACEMENT_3D ( 'NONE', #9919, #594, #1364 ) ;
#7117 = DIRECTION ( 'NONE',  ( 0.000000000000000000, -1.000000000000000000, 0.000000000000000000 ) ) ;
#7118 = PLANE ( 'NONE',  #9741 ) ;
#7119 =( BOUNDED_CURVE ( )  B_SPLINE_CURVE ( 2, ( #1885, #6747, #952, #230, #2003, #9562, #1942, #3646, #10389 ),
 .UNSPECIFIED., .F., .F. ) 
 B_SPLINE_CURVE_WITH_KNOTS ( ( 3, 2, 2, 2, 3 ),
 ( 0.3500000000000000333, 0.3750000000000000555, 0.4000000000000000222, 0.4249999999999999889, 0.4500000000000000111 ),
 .UNSPECIFIED. ) 
 CURVE ( )  GEOMETRIC_REPRESENTATION_ITEM ( )  RATIONAL_B_SPLINE_CURVE ( ( 0.9999999999999997780, 0.9238795325112869605, 1.000000000000000000, 0.9238795325112867385, 1.000000000000000000, 0.9238795325112867385, 1.000000000000000000, 0.9238795325112867385, 1.000000000000000000 ) ) 
 REPRESENTATION_ITEM ( '' )  );
#7120 = ORIENTED_EDGE ( 'NONE', *, *, #7810, .F. ) ;
#7121 = VECTOR ( 'NONE', #980, 1000.000000000000000 ) ;
#7122 = VECTOR ( 'NONE', #3228, 1000.000000000000000 ) ;
#7123 = ORIENTED_EDGE ( 'NONE', *, *, #2864, .T. ) ;
#7124 = CARTESIAN_POINT ( 'NONE',  ( -24.62111388750000174, 2.893749999044084475, -3.015216831376932151E-15 ) ) ;
#7125 = DIRECTION ( 'NONE',  ( 0.000000000000000000, 0.000000000000000000, 1.000000000000000000 ) ) ;
#7126 = VECTOR ( 'NONE', #927, 1000.000000000000114 ) ;
#7127 = CARTESIAN_POINT ( 'NONE',  ( 7.171633369868234631, 7.781088913245556959, 11.42163336986834388 ) ) ;
#7128 = FACE_OUTER_BOUND ( 'NONE', #6078, .T. ) ;
#7129 = FACE_OUTER_BOUND ( 'NONE', #6872, .T. ) ;
#7130 = AXIS2_PLACEMENT_3D ( 'NONE', #6253, #9557, #7791 ) ;
#7131 = ORIENTED_EDGE ( 'NONE', *, *, #8143, .F. ) ;
#7132 = EDGE_CURVE ( 'NONE', #4029, #7313, #3297, .T. ) ;
#7133 = AXIS2_PLACEMENT_3D ( 'NONE', #2073, #5450, #1202 ) ;
#7134 = ORIENTED_EDGE ( 'NONE', *, *, #1127, .F. ) ;
#7135 = ADVANCED_FACE ( 'NONE', ( #1603 ), #6863, .T. ) ;
#7136 = CARTESIAN_POINT ( 'NONE',  ( 24.62111388749999463, 5.331249999044085364, 10.19839929293507730 ) ) ;
#7137 = DIRECTION ( 'NONE',  ( 0.000000000000000000, 0.000000000000000000, 1.000000000000000000 ) ) ;
#7138 = AXIS2_PLACEMENT_3D ( 'NONE', #1362, #8158, #5512 ) ;
#7139 = CARTESIAN_POINT ( 'NONE',  ( 10.19839929293506486, 1.206249999044084698, 24.62111388749999819 ) ) ;
#7140 = VERTEX_POINT ( 'NONE', #2531 ) ;
#7141 = LINE ( 'NONE', #10500, #6012 ) ;
#7142 = ADVANCED_FACE ( 'NONE', ( #8392 ), #3771, .T. ) ;
#7143 = DIRECTION ( 'NONE',  ( 0.000000000000000000, -2.775557561562887961E-17, -1.000000000000000000 ) ) ;
#7144 = CARTESIAN_POINT ( 'NONE',  ( -24.62111388750000884, 3.781249999044084653, 10.19839929293505421 ) ) ;
#7145 = CARTESIAN_POINT ( 'NONE',  ( -12.47307621135344391, 28.00000000000000000, -15.60400172474256131 ) ) ;
#7146 = VERTEX_POINT ( 'NONE', #5156 ) ;
#7147 = ORIENTED_EDGE ( 'NONE', *, *, #8610, .F. ) ;
#7148 = ADVANCED_FACE ( 'NONE', ( #4261 ), #4323, .F. ) ;
#7149 = CARTESIAN_POINT ( 'NONE',  ( -0.3335819196118727237, 19.34316356887877930, -6.994037468151971026 ) ) ;
#7150 = CARTESIAN_POINT ( 'NONE',  ( -24.62111388750000174, 3.656249999044084653, -10.19839929293506131 ) ) ;
#7151 = CARTESIAN_POINT ( 'NONE',  ( 10.19839929293505953, 1.581249999044084475, -24.62111388750000174 ) ) ;
#7152 = CARTESIAN_POINT ( 'NONE',  ( 1.530808498934191521E-15, 4.250000000000000000, -25.00000000000000000 ) ) ;
#7153 = ADVANCED_FACE ( 'NONE', ( #6809, #836 ), #10221, .T. ) ;
#7154 = FACE_OUTER_BOUND ( 'NONE', #4671, .T. ) ;
#7155 = CARTESIAN_POINT ( 'NONE',  ( 0.000000000000000000, 82.00000000000000000, 0.000000000000000000 ) ) ;
#7156 = CARTESIAN_POINT ( 'NONE',  ( -10.47307621135315792, 28.00000000000000000, 12.13990010960504762 ) ) ;
#7157 = CARTESIAN_POINT ( 'NONE',  ( -10.35533905932737575, 2.312500000000000888, -25.00000000000000000 ) ) ;
#7158 = ORIENTED_EDGE ( 'NONE', *, *, #8125, .F. ) ;
#7159 = ORIENTED_EDGE ( 'NONE', *, *, #4669, .T. ) ;
#7160 = PRODUCT_DEFINITION_SHAPE ( 'NONE', 'NONE',  #10951 ) ;
#7161 = ORIENTED_EDGE ( 'NONE', *, *, #3435, .F. ) ;
#7162 = DIRECTION ( 'NONE',  ( 0.000000000000000000, 1.000000000000000000, 0.000000000000000000 ) ) ;
#7163 = EDGE_CURVE ( 'NONE', #5240, #8662, #7743, .T. ) ;
#7164 = CARTESIAN_POINT ( 'NONE',  ( 0.000000000000000000, 0.000000000000000000, 0.000000000000000000 ) ) ;
#7165 = DIRECTION ( 'NONE',  ( 0.000000000000000000, 1.000000000000000000, 0.000000000000000000 ) ) ;
#7166 = DIRECTION ( 'NONE',  ( 1.000000000000000000, 0.000000000000000000, 0.000000000000000000 ) ) ;
#7167 = CARTESIAN_POINT ( 'NONE',  ( 2.449293598294706414E-16, 20.00000000000000355, 2.000000000000000000 ) ) ;
#7168 = CARTESIAN_POINT ( 'NONE',  ( -4.592425496802574367E-15, 3.750000000000000000, 25.00000000000000000 ) ) ;
#7169 = ORIENTED_EDGE ( 'NONE', *, *, #9789, .T. ) ;
#7170 = EDGE_LOOP ( 'NONE', ( #5133, #5813, #8233, #3246 ) ) ;
#7171 = ORIENTED_EDGE ( 'NONE', *, *, #4857, .T. ) ;
#7172 = ADVANCED_FACE ( 'NONE', ( #4204 ), #959, .F. ) ;
#7173 = DIRECTION ( 'NONE',  ( 0.000000000000000000, 0.000000000000000000, -1.000000000000000000 ) ) ;
#7174 = CARTESIAN_POINT ( 'NONE',  ( 7.874999999999916511, -0.001000000000001000089, -13.63990010960495702 ) ) ;
#7175 = DIRECTION ( 'NONE',  ( -0.000000000000000000, 1.000000000000000000, -0.000000000000000000 ) ) ;
#7176 = DIRECTION ( 'NONE',  ( -0.000000000000000000, 1.000000000000000000, -0.000000000000000000 ) ) ;
#7177 = CARTESIAN_POINT ( 'NONE',  ( -19.75000000000000000, 25.00000000000000000, 2.108281996628241301E-13 ) ) ;
#7178 = EDGE_LOOP ( 'NONE', ( #6467, #5505, #4751, #5767, #1326, #10283 ) ) ;
#7179 = EDGE_LOOP ( 'NONE', ( #2709, #2210, #4687, #8586 ) ) ;
#7180 = DIRECTION ( 'NONE',  ( -1.000000000000000000, -0.000000000000000000, -0.000000000000000000 ) ) ;
#7181 = DIRECTION ( 'NONE',  ( 0.000000000000000000, 0.000000000000000000, -1.000000000000000000 ) ) ;
#7182 = CARTESIAN_POINT ( 'NONE',  ( 24.62111388749999108, 4.331249999044084475, 10.19839929293507730 ) ) ;
#7183 = ORIENTED_EDGE ( 'NONE', *, *, #8538, .F. ) ;
#7184 = CARTESIAN_POINT ( 'NONE',  ( 0.000000000000000000, 20.00000000000000355, -4.999999999999997335 ) ) ;
#7185 =( NAMED_UNIT ( * ) PLANE_ANGLE_UNIT ( ) SI_UNIT ( $, .RADIAN. ) );
#7186 = CARTESIAN_POINT ( 'NONE',  ( 7.347880794884120722E-16, 82.00000000000000000, -6.000000000000000888 ) ) ;
#7187 = CARTESIAN_POINT ( 'NONE',  ( 24.62111388750000174, 4.218749999044084653, 0.000000000000000000 ) ) ;
#7188 = ORIENTED_EDGE ( 'NONE', *, *, #1807, .F. ) ;
#7189 = ORIENTED_EDGE ( 'NONE', *, *, #7955, .F. ) ;
#7190 = VERTEX_POINT ( 'NONE', #6754 ) ;
#7191 = CIRCLE ( 'NONE', #9666, 25.00000000000000000 ) ;
#7192 = CARTESIAN_POINT ( 'NONE',  ( -10.19839929293507552, 2.906249999044085541, 24.62111388749999463 ) ) ;
#7193 = CARTESIAN_POINT ( 'NONE',  ( -4.522825247065398226E-15, 2.143749999044084920, 24.62111388750000174 ) ) ;
#7194 = ORIENTED_EDGE ( 'NONE', *, *, #323, .F. ) ;
#7195 = CARTESIAN_POINT ( 'NONE',  ( -17.67766952966369232, 1.625000000000000222, 17.67766952966368876 ) ) ;
#7196 = ADVANCED_FACE ( 'NONE', ( #2639 ), #3418, .T. ) ;
#7197 = EDGE_CURVE ( 'NONE', #2830, #4148, #1465, .T. ) ;
#7198 = DIRECTION ( 'NONE',  ( 0.000000000000000000, 0.000000000000000000, -1.000000000000000000 ) ) ;
#7199 = CARTESIAN_POINT ( 'NONE',  ( 1.530808498934191521E-15, 0.8624999980881691286, -25.00000000000000000 ) ) ;
#7200 = EDGE_CURVE ( 'NONE', #5087, #8288, #4654, .T. ) ;
#7201 = FACE_OUTER_BOUND ( 'NONE', #10137, .T. ) ;
#7202 = CARTESIAN_POINT ( 'NONE',  ( 11.06217782649105175, 10.00000000000000355, 6.386751345948189496 ) ) ;
#7203 = AXIS2_PLACEMENT_3D ( 'NONE', #5965, #46, #10156 ) ;
#7204 = ORIENTED_EDGE ( 'NONE', *, *, #8543, .T. ) ;
#7205 = EDGE_CURVE ( 'NONE', #1064, #9664, #5225, .T. ) ;
#7206 = FACE_OUTER_BOUND ( 'NONE', #1546, .T. ) ;
#7207 = DIRECTION ( 'NONE',  ( 1.000000000000000000, 0.000000000000000000, 0.000000000000000000 ) ) ;
#7208 = AXIS2_PLACEMENT_3D ( 'NONE', #124, #9232, #4270 ) ;
#7209 = DIRECTION ( 'NONE',  ( 0.000000000000000000, 0.000000000000000000, 1.000000000000000000 ) ) ;
#7210 = EDGE_CURVE ( 'NONE', #856, #3713, #1823, .T. ) ;
#7211 = LINE ( 'NONE', #7359, #7630 ) ;
#7212 = CARTESIAN_POINT ( 'NONE',  ( 7.276923788646575630, -0.001000000000001000089, -18.60400172474270519 ) ) ;
#7213 = PLANE ( 'NONE',  #7082 ) ;
#7214 = DIRECTION ( 'NONE',  ( 0.000000000000000000, 0.000000000000000000, 1.000000000000000000 ) ) ;
#7215 = EDGE_CURVE ( 'NONE', #1720, #544, #1296, .T. ) ;
#7216 = ORIENTED_EDGE ( 'NONE', *, *, #8768, .T. ) ;
#7217 = CARTESIAN_POINT ( 'NONE',  ( 12.92820323027550700, 10.00000000000000355, -0.1339745962155138304 ) ) ;
#7218 = CARTESIAN_POINT ( 'NONE',  ( 3.957930336368489021E-15, -0.001000000000001000089, 22.75000000000000000 ) ) ;
#7219 = CARTESIAN_POINT ( 'NONE',  ( 4.946152422706616036, 10.00000000000000355, 3.433012701892241836 ) ) ;
#7220 = LINE ( 'NONE', #8049, #10643 ) ;
#7221 = CYLINDRICAL_SURFACE ( 'NONE', #9396, 5.999999999999999112 ) ;
#7222 = ORIENTED_EDGE ( 'NONE', *, *, #7378, .F. ) ;
#7223 = EDGE_LOOP ( 'NONE', ( #9472, #1700, #9167, #3806, #9777, #6270 ) ) ;
#7224 = CIRCLE ( 'NONE', #2453, 20.00000000000000000 ) ;
#7225 = CARTESIAN_POINT ( 'NONE',  ( 3.061616997868383043E-15, 85.00000000000000000, 25.00000000000000000 ) ) ;
#7226 = DIRECTION ( 'NONE',  ( -0.4999999999999888423, 0.000000000000000000, -0.8660254037844449249 ) ) ;
#7227 = CARTESIAN_POINT ( 'NONE',  ( 17.40975659021752975, 2.518749999044084475, -17.40975659021752975 ) ) ;
#7228 = EDGE_LOOP ( 'NONE', ( #9074, #10340, #10511, #1093 ) ) ;
#7229 = CARTESIAN_POINT ( 'NONE',  ( 0.000000000000000000, 85.00000000000000000, 25.00000000000000000 ) ) ;
#7230 = DIRECTION ( 'NONE',  ( 0.000000000000000000, 0.000000000000000000, -1.000000000000000000 ) ) ;
#7231 = ORIENTED_EDGE ( 'NONE', *, *, #9421, .F. ) ;
#7232 = CARTESIAN_POINT ( 'NONE',  ( -24.62111388750000174, 1.718749999044084431, -3.015216831376932151E-15 ) ) ;
#7233 = LINE ( 'NONE', #8897, #664 ) ;
#7234 = EDGE_CURVE ( 'NONE', #416, #5054, #10495, .T. ) ;
#7235 = ORIENTED_EDGE ( 'NONE', *, *, #3491, .F. ) ;
#7236 = AXIS2_PLACEMENT_3D ( 'NONE', #9306, #10370, #6963 ) ;
#7237 = VERTEX_POINT ( 'NONE', #4558 ) ;
#7238 = AXIS2_PLACEMENT_3D ( 'NONE', #1833, #10050, #3412 ) ;
#7239 = ORIENTED_EDGE ( 'NONE', *, *, #1147, .F. ) ;
#7240 = VERTEX_POINT ( 'NONE', #10395 ) ;
#7241 = PRODUCT_RELATED_PRODUCT_CATEGORY ( 'part', '', ( #451 ) ) ;
#7242 = CARTESIAN_POINT ( 'NONE',  ( -24.62111388750000884, 4.781249999044083765, 10.19839929293505421 ) ) ;
#7243 = CARTESIAN_POINT ( 'NONE',  ( 24.62111388750000174, 1.393749999044084475, 0.000000000000000000 ) ) ;
#7244 = CARTESIAN_POINT ( 'NONE',  ( 17.67766952966369232, 4.125000000000000000, -17.67766952966369232 ) ) ;
#7245 = AXIS2_PLACEMENT_3D ( 'NONE', #8804, #10306, #8700 ) ;
#7246 = AXIS2_PLACEMENT_3D ( 'NONE', #2092, #7960, #9717 ) ;
#7247 = DIRECTION ( 'NONE',  ( 1.000000000000000000, 0.000000000000000000, 0.000000000000000000 ) ) ;
#7248 = DIRECTION ( 'NONE',  ( 0.000000000000000000, 0.000000000000000000, 1.000000000000000000 ) ) ;
#7249 = CARTESIAN_POINT ( 'NONE',  ( 1.530808498934191521E-15, 3.250000000000000444, -25.00000000000000000 ) ) ;
#7250 = EDGE_LOOP ( 'NONE', ( #1688, #3177, #4002, #914 ) ) ;
#7251 = EDGE_LOOP ( 'NONE', ( #5405, #3425, #9325, #10830, #4419 ) ) ;
#7252 = EDGE_CURVE ( 'NONE', #417, #10229, #6064, .T. ) ;
#7253 = AXIS2_PLACEMENT_3D ( 'NONE', #8698, #3553, #10355 ) ;
#7254 = LINE ( 'NONE', #2989, #1242 ) ;
#7255 = DIRECTION ( 'NONE',  ( 0.000000000000000000, -0.8660254037844387076, -0.5000000000000001110 ) ) ;
#7256 = CARTESIAN_POINT ( 'NONE',  ( 2.999999999999996447, 28.00000000000000000, -19.75000000000000000 ) ) ;
#7257 = CARTESIAN_POINT ( 'NONE',  ( 0.000000000000000000, 85.00000000000000000, -28.00000000000000000 ) ) ;
#7258 = EDGE_CURVE ( 'NONE', #9966, #10861, #7450, .T. ) ;
#7259 = DIRECTION ( 'NONE',  ( 0.000000000000000000, 0.000000000000000000, -1.000000000000000000 ) ) ;
#7260 = PLANE ( 'NONE',  #8831 ) ;
#7261 = LINE ( 'NONE', #4739, #9039 ) ;
#7262 = VECTOR ( 'NONE', #4833, 1000.000000000000000 ) ;
#7263 = ORIENTED_EDGE ( 'NONE', *, *, #2241, .F. ) ;
#7264 = ADVANCED_FACE ( 'NONE', ( #4610, #2910 ), #1067, .F. ) ;
#7265 = AXIS2_PLACEMENT_3D ( 'NONE', #10216, #4941, #110 ) ;
#7266 = ORIENTED_EDGE ( 'NONE', *, *, #1676, .T. ) ;
#7267 = FACE_OUTER_BOUND ( 'NONE', #3559, .T. ) ;
#7268 = DIRECTION ( 'NONE',  ( 0.000000000000000000, 2.775557561562888270E-17, 1.000000000000000000 ) ) ;
#7269 = EDGE_CURVE ( 'NONE', #6293, #8354, #10292, .T. ) ;
#7270 = CARTESIAN_POINT ( 'NONE',  ( 17.67766952966368521, 4.487499998088169129, 17.67766952966369232 ) ) ;
#7271 = DIRECTION ( 'NONE',  ( 0.000000000000000000, 1.000000000000000000, 0.000000000000000000 ) ) ;
#7272 = DIRECTION ( 'NONE',  ( 0.000000000000000000, 0.000000000000000000, 1.000000000000000000 ) ) ;
#7273 = VECTOR ( 'NONE', #3406, 1000.000000000000000 ) ;
#7274 = AXIS2_PLACEMENT_3D ( 'NONE', #304, #9590, #8703 ) ;
#7275 = VERTEX_POINT ( 'NONE', #10343 ) ;
#7276 = VERTEX_POINT ( 'NONE', #2008 ) ;
#7277 = AXIS2_PLACEMENT_3D ( 'NONE', #756, #4803, #2400 ) ;
#7278 =( NAMED_UNIT ( * ) SI_UNIT ( $, .STERADIAN. ) SOLID_ANGLE_UNIT ( ) );
#7279 = CARTESIAN_POINT ( 'NONE',  ( -6.062177826491100596, 20.00000000000000355, 3.499999999999942712 ) ) ;
#7280 = DIRECTION ( 'NONE',  ( -1.000000000000000000, -0.000000000000000000, -7.228014483236695816E-17 ) ) ;
#7281 = EDGE_CURVE ( 'NONE', #2972, #7713, #5427, .T. ) ;
#7282 = VERTEX_POINT ( 'NONE', #10449 ) ;
#7283 = DIRECTION ( 'NONE',  ( -0.8660254037844407060, 0.4999999999999965583, -0.000000000000000000 ) ) ;
#7284 = CARTESIAN_POINT ( 'NONE',  ( 0.000000000000000000, 0.000000000000000000, 0.000000000000000000 ) ) ;
#7285 = DIRECTION ( 'NONE',  ( 0.000000000000000000, 0.000000000000000000, 1.000000000000000000 ) ) ;
#7286 = EDGE_LOOP ( 'NONE', ( #3450, #6182, #6511, #2383 ) ) ;
#7287 = VECTOR ( 'NONE', #6365, 1000.000000000000000 ) ;
#7288 = CARTESIAN_POINT ( 'NONE',  ( 17.40975659021752620, 4.093749999044084653, 17.40975659021753330 ) ) ;
#7289 = CARTESIAN_POINT ( 'NONE',  ( 24.62111388750000174, 1.281249999044084653, -10.19839929293505776 ) ) ;
#7290 = VECTOR ( 'NONE', #8098, 1000.000000000000000 ) ;
#7291 = EDGE_LOOP ( 'NONE', ( #1184, #6081, #6697, #9465 ) ) ;
#7292 = VERTEX_POINT ( 'NONE', #8741 ) ;
#7293 = VECTOR ( 'NONE', #3004, 999.9999999999998863 ) ;
#7294 = CARTESIAN_POINT ( 'NONE',  ( -25.00000000000000000, 3.112499998088169129, -3.061616997868383043E-15 ) ) ;
#7295 = FACE_OUTER_BOUND ( 'NONE', #4845, .T. ) ;
#7296 = CARTESIAN_POINT ( 'NONE',  ( -17.40975659021753330, 4.018749999044084475, 17.40975659021752975 ) ) ;
#7297 = ORIENTED_EDGE ( 'NONE', *, *, #5455, .T. ) ;
#7298 = DIRECTION ( 'NONE',  ( 0.000000000000000000, 1.000000000000000000, 0.000000000000000000 ) ) ;
#7299 = CARTESIAN_POINT ( 'NONE',  ( 0.000000000000000000, 1.000000000000001998, 0.5773502691896277295 ) ) ;
#7300 = CARTESIAN_POINT ( 'NONE',  ( 0.000000000000000000, 0.000000000000000000, 0.000000000000000000 ) ) ;
#7301 = DIRECTION ( 'NONE',  ( 0.000000000000000000, -1.000000000000000000, 0.000000000000000000 ) ) ;
#7302 = VERTEX_POINT ( 'NONE', #7186 ) ;
#7303 = VERTEX_POINT ( 'NONE', #6307 ) ;
#7304 = VERTEX_POINT ( 'NONE', #1180 ) ;
#7305 = CARTESIAN_POINT ( 'NONE',  ( 17.67766952966368521, 3.875000000000000000, 17.67766952966369232 ) ) ;
#7306 = DIRECTION ( 'NONE',  ( 0.000000000000000000, 0.000000000000000000, 1.000000000000000000 ) ) ;
#7307 = CARTESIAN_POINT ( 'NONE',  ( 17.67766952966368521, 1.487499998088169129, 17.67766952966369232 ) ) ;
#7308 = CARTESIAN_POINT ( 'NONE',  ( 0.000000000000000000, 5.000000000000000000, 0.000000000000000000 ) ) ;
#7309 = DIRECTION ( 'NONE',  ( -0.4330127018922192428, 0.8660254037844380415, -0.2500000000000026645 ) ) ;
#7310 = ADVANCED_FACE ( 'NONE', ( #7915 ), #343, .T. ) ;
#7311 = CARTESIAN_POINT ( 'NONE',  ( -24.62111388750000884, 1.781249999044084431, 10.19839929293505421 ) ) ;
#7312 = DIRECTION ( 'NONE',  ( -0.000000000000000000, -1.000000000000000000, -0.000000000000000000 ) ) ;
#7313 = VERTEX_POINT ( 'NONE', #10551 ) ;
#7314 = EDGE_CURVE ( 'NONE', #122, #3225, #6263, .T. ) ;
#7315 = ORIENTED_EDGE ( 'NONE', *, *, #6802, .T. ) ;
#7316 = DIRECTION ( 'NONE',  ( 0.000000000000000000, 0.000000000000000000, -1.000000000000000000 ) ) ;
#7317 = DIRECTION ( 'NONE',  ( 0.000000000000000000, 0.000000000000000000, -1.000000000000000000 ) ) ;
#7318 = CARTESIAN_POINT ( 'NONE',  ( 1.499999999999999556, 83.00000000000000000, -1.500000000000000222 ) ) ;
#7319 = EDGE_CURVE ( 'NONE', #1247, #5192, #2053, .T. ) ;
#7320 = DIRECTION ( 'NONE',  ( 0.000000000000000000, -0.000000000000000000, 1.000000000000000000 ) ) ;
#7321 = ADVANCED_FACE ( 'NONE', ( #3765 ), #1891, .T. ) ;
#7322 = FACE_OUTER_BOUND ( 'NONE', #8137, .T. ) ;
#7323 = EDGE_CURVE ( 'NONE', #544, #1720, #4836, .T. ) ;
#7324 = ORIENTED_EDGE ( 'NONE', *, *, #2666, .T. ) ;
#7325 = EDGE_CURVE ( 'NONE', #122, #1858, #4663, .T. ) ;
#7326 = EDGE_LOOP ( 'NONE', ( #8072, #1333, #5649 ) ) ;
#7327 = DIRECTION ( 'NONE',  ( -1.000000000000000000, 0.000000000000000000, 1.069128445102650095E-14 ) ) ;
#7328 = CARTESIAN_POINT ( 'NONE',  ( 18.60400172474263414, 28.00000000000000000, -7.276923788646775471 ) ) ;
#7329 = CARTESIAN_POINT ( 'NONE',  ( 24.62111388750000174, 4.456249999044084475, -10.19839929293505776 ) ) ;
#7330 = VERTEX_POINT ( 'NONE', #9931 ) ;
#7331 = CARTESIAN_POINT ( 'NONE',  ( 17.67766952966369232, 3.737499998088169573, -17.67766952966369232 ) ) ;
#7332 = SHAPE_DEFINITION_REPRESENTATION ( #10416, #9997 ) ;
#7333 = FACE_OUTER_BOUND ( 'NONE', #5038, .T. ) ;
#7334 = ORIENTED_EDGE ( 'NONE', *, *, #5735, .T. ) ;
#7335 = DIRECTION ( 'NONE',  ( -0.7559289460184509535, -0.000000000000000000, -0.6546536707079810835 ) ) ;
#7336 = EDGE_CURVE ( 'NONE', #8103, #257, #243, .T. ) ;
#7337 = CARTESIAN_POINT ( 'NONE',  ( 1.507608415688466075E-15, 0.4687499990440845421, -24.62111388750000174 ) ) ;
#7338 = ORIENTED_EDGE ( 'NONE', *, *, #5837, .T. ) ;
#7339 = ORIENTED_EDGE ( 'NONE', *, *, #2196, .T. ) ;
#7340 = ORIENTED_EDGE ( 'NONE', *, *, #4770, .T. ) ;
#7341 = ADVANCED_FACE ( 'NONE', ( #6570, #2365 ), #708, .F. ) ;
#7342 = CARTESIAN_POINT ( 'NONE',  ( -10.35533905932739174, 5.299999998088169129, 24.99999999999999289 ) ) ;
#7343 = CARTESIAN_POINT ( 'NONE',  ( 82.32050807568876394, 89.28203230275514102, 0.000000000000000000 ) ) ;
#7344 = CARTESIAN_POINT ( 'NONE',  ( 24.62111388750000174, 3.281249999044085097, -10.19839929293505776 ) ) ;
#7345 = VERTEX_POINT ( 'NONE', #10664 ) ;
#7346 = CARTESIAN_POINT ( 'NONE',  ( 8.660254037844401509, 95.00000000000001421, 5.000000000000000000 ) ) ;
#7347 = CARTESIAN_POINT ( 'NONE',  ( -25.00000000000000000, 2.112499998088169129, -3.061616997868383043E-15 ) ) ;
#7348 = DIRECTION ( 'NONE',  ( 0.000000000000000000, -1.000000000000000000, 0.000000000000000000 ) ) ;
#7349 = DIRECTION ( 'NONE',  ( -0.000000000000000000, -1.000000000000000000, -0.000000000000000000 ) ) ;
#7350 = DIRECTION ( 'NONE',  ( -0.000000000000000000, -1.000000000000000000, -0.000000000000000000 ) ) ;
#7351 = STYLED_ITEM ( 'NONE', ( #7863 ), #4934 ) ;
#7352 = ORIENTED_EDGE ( 'NONE', *, *, #6186, .T. ) ;
#7353 = ORIENTED_EDGE ( 'NONE', *, *, #6061, .T. ) ;
#7354 = ORIENTED_EDGE ( 'NONE', *, *, #5259, .F. ) ;
#7355 = EDGE_CURVE ( 'NONE', #811, #9751, #3120, .T. ) ;
#7356 = CARTESIAN_POINT ( 'NONE',  ( 17.40975659021752975, 2.343749999044085097, -17.40975659021752975 ) ) ;
#7357 = DIRECTION ( 'NONE',  ( 0.000000000000000000, -0.5000000000000001110, 0.8660254037844387076 ) ) ;
#7358 = ORIENTED_EDGE ( 'NONE', *, *, #3248, .F. ) ;
#7359 = CARTESIAN_POINT ( 'NONE',  ( 3.061616997868383043E-15, 5.000000000000000000, 25.00000000000000000 ) ) ;
#7360 = DIRECTION ( 'NONE',  ( 0.000000000000000000, 1.000000000000000000, 0.000000000000000000 ) ) ;
#7361 = VECTOR ( 'NONE', #6700, 1000.000000000000000 ) ;
#7362 = CARTESIAN_POINT ( 'NONE',  ( -10.19839929293505776, 3.531249999044084653, -24.62111388750000174 ) ) ;
#7363 = CARTESIAN_POINT ( 'NONE',  ( -25.00000000000000000, 3.500000000000000000, -3.061616997868383043E-15 ) ) ;
#7364 = ORIENTED_EDGE ( 'NONE', *, *, #1952, .F. ) ;
#7365 = ORIENTED_EDGE ( 'NONE', *, *, #4714, .F. ) ;
#7366 = VECTOR ( 'NONE', #9347, 1000.000000000000000 ) ;
#7367 = EDGE_LOOP ( 'NONE', ( #7983, #2953 ) ) ;
#7368 = ORIENTED_EDGE ( 'NONE', *, *, #9031, .F. ) ;
#7369 = CIRCLE ( 'NONE', #5983, 2.999999999999999112 ) ;
#7370 = LINE ( 'NONE', #5457, #4649 ) ;
#7371 = DIRECTION ( 'NONE',  ( 0.000000000000000000, 0.000000000000000000, -1.000000000000000000 ) ) ;
#7372 = DIRECTION ( 'NONE',  ( -0.000000000000000000, 1.000000000000000000, -0.000000000000000000 ) ) ;
#7373 = FACE_OUTER_BOUND ( 'NONE', #5952, .T. ) ;
#7374 = DIRECTION ( 'NONE',  ( 1.000000000000000000, 0.000000000000000000, 0.000000000000000000 ) ) ;
#7375 = VERTEX_POINT ( 'NONE', #3983 ) ;
#7376 = ADVANCED_FACE ( 'NONE', ( #7333 ), #1487, .F. ) ;
#7377 =( BOUNDED_CURVE ( )  B_SPLINE_CURVE ( 2, ( #10721, #7565, #8561, #5269, #5218, #9393, #3314, #4203, #5093 ),
 .UNSPECIFIED., .F., .F. ) 
 B_SPLINE_CURVE_WITH_KNOTS ( ( 3, 2, 2, 2, 3 ),
 ( 0.6500000000000000222, 0.6750000000000000444, 0.6999999999999999556, 0.7249999999999999778, 0.7500000000000000000 ),
 .UNSPECIFIED. ) 
 CURVE ( )  GEOMETRIC_REPRESENTATION_ITEM ( )  RATIONAL_B_SPLINE_CURVE ( ( 1.000000000000000000, 0.9238795325112867385, 1.000000000000000000, 0.9238795325112867385, 1.000000000000000000, 0.9238795325112867385, 1.000000000000000000, 0.9238795325112867385, 1.000000000000000000 ) ) 
 REPRESENTATION_ITEM ( '' )  );
#7378 = EDGE_CURVE ( 'NONE', #3294, #2327, #3775, .T. ) ;
#7379 = EDGE_CURVE ( 'NONE', #1334, #5377, #9417, .T. ) ;
#7380 = CARTESIAN_POINT ( 'NONE',  ( -1.500000000000000444, 88.00000000000001421, -1.500000000000000222 ) ) ;
#7381 = CARTESIAN_POINT ( 'NONE',  ( -24.62111388750000174, 3.893749999044084475, -3.015216831376932151E-15 ) ) ;
#7382 = ORIENTED_EDGE ( 'NONE', *, *, #9098, .T. ) ;
#7383 = CARTESIAN_POINT ( 'NONE',  ( 6.999999999999997335, 20.00000000000000355, 3.024924061234557371E-14 ) ) ;
#7384 = DIRECTION ( 'NONE',  ( 1.000000000000000000, 0.000000000000000000, 0.000000000000000000 ) ) ;
#7385 = DIRECTION ( 'NONE',  ( 0.000000000000000000, -0.000000000000000000, -1.000000000000000000 ) ) ;
#7386 = ORIENTED_EDGE ( 'NONE', *, *, #10158, .F. ) ;
#7387 = FACE_OUTER_BOUND ( 'NONE', #5143, .T. ) ;
#7388 = CARTESIAN_POINT ( 'NONE',  ( -4.522825247065398226E-15, 1.968749999044084653, 24.62111388750000174 ) ) ;
#7389 = EDGE_CURVE ( 'NONE', #8219, #10861, #6419, .T. ) ;
#7390 = ORIENTED_EDGE ( 'NONE', *, *, #6014, .F. ) ;
#7391 = VERTEX_POINT ( 'NONE', #1373 ) ;
#7392 = ORIENTED_EDGE ( 'NONE', *, *, #4234, .F. ) ;
#7393 = CONICAL_SURFACE ( 'NONE', #3731, 22.18092213764227694, 0.3490658503988666728 ) ;
#7394 = CIRCLE ( 'NONE', #2625, 28.00000000000000000 ) ;
#7395 = EDGE_CURVE ( 'NONE', #7827, #2098, #4672, .T. ) ;
#7396 = CARTESIAN_POINT ( 'NONE',  ( 24.62111388749999463, 1.331249999044084475, 10.19839929293507730 ) ) ;
#7397 = DIRECTION ( 'NONE',  ( -0.000000000000000000, 0.000000000000000000, 1.000000000000000000 ) ) ;
#7398 = CARTESIAN_POINT ( 'NONE',  ( 24.62111388749999463, 1.156249999044084431, 10.19839929293507730 ) ) ;
#7399 = DIRECTION ( 'NONE',  ( 0.000000000000000000, 0.000000000000000000, 1.000000000000000000 ) ) ;
#7400 = LINE ( 'NONE', #1604, #7548 ) ;
#7401 = CARTESIAN_POINT ( 'NONE',  ( 7.276923788646707969, -0.001000000000001000089, 18.60400172474265190 ) ) ;
#7402 = LINE ( 'NONE', #1606, #7984 ) ;
#7403 = DIRECTION ( 'NONE',  ( 0.000000000000000000, -1.000000000000000000, 0.000000000000000000 ) ) ;
#7404 = EDGE_CURVE ( 'NONE', #6450, #10325, #276, .T. ) ;
#7405 = AXIS2_PLACEMENT_3D ( 'NONE', #7671, #5960, #1648 ) ;
#7406 = CIRCLE ( 'NONE', #2630, 2.149999999999999911 ) ;
#7407 = FACE_OUTER_BOUND ( 'NONE', #6742, .T. ) ;
#7408 = ORIENTED_EDGE ( 'NONE', *, *, #7904, .F. ) ;
#7409 = ORIENTED_EDGE ( 'NONE', *, *, #791, .F. ) ;
#7410 = VERTEX_POINT ( 'NONE', #6515 ) ;
#7411 = ORIENTED_EDGE ( 'NONE', *, *, #1715, .T. ) ;
#7412 = VECTOR ( 'NONE', #5303, 1000.000000000000114 ) ;
#7413 = VECTOR ( 'NONE', #10703, 1000.000000000000000 ) ;
#7414 = DIRECTION ( 'NONE',  ( 0.000000000000000000, -1.000000000000000000, 0.000000000000000000 ) ) ;
#7415 = LINE ( 'NONE', #9235, #4911 ) ;
#7416 = EDGE_CURVE ( 'NONE', #7292, #1671, #6079, .T. ) ;
#7417 = ORIENTED_EDGE ( 'NONE', *, *, #319, .F. ) ;
#7418 = DIRECTION ( 'NONE',  ( -0.000000000000000000, -1.000000000000000000, -0.000000000000000000 ) ) ;
#7419 = DIRECTION ( 'NONE',  ( 0.000000000000000000, 1.000000000000000000, 9.470910429910644418E-17 ) ) ;
#7420 = DIRECTION ( 'NONE',  ( 0.000000000000000000, 0.000000000000000000, -1.000000000000000000 ) ) ;
#7421 = CARTESIAN_POINT ( 'NONE',  ( 17.40975659021752975, 3.343749999044085097, -17.40975659021752975 ) ) ;
#7422 = CARTESIAN_POINT ( 'NONE',  ( 0.000000000000000000, 20.00000000000000355, 0.000000000000000000 ) ) ;
#7423 = CIRCLE ( 'NONE', #2648, 2.999999999999997335 ) ;
#7424 = ORIENTED_EDGE ( 'NONE', *, *, #2873, .T. ) ;
#7425 = VECTOR ( 'NONE', #3151, 1000.000000000000114 ) ;
#7426 = ORIENTED_EDGE ( 'NONE', *, *, #1345, .F. ) ;
#7427 = CARTESIAN_POINT ( 'NONE',  ( 3.429011037612589276E-15, 0.000000000000000000, 28.00000000000000000 ) ) ;
#7428 = DIRECTION ( 'NONE',  ( 0.000000000000000000, -1.000000000000000000, 0.000000000000000000 ) ) ;
#7429 = CARTESIAN_POINT ( 'NONE',  ( -7.875000000000116351, -0.001000000000001000089, -13.63990010960484334 ) ) ;
#7430 = AXIS2_PLACEMENT_3D ( 'NONE', #3804, #3537, #6351 ) ;
#7431 = CARTESIAN_POINT ( 'NONE',  ( 24.99999999999999289, 3.937500000000000000, 10.35533905932739529 ) ) ;
#7432 = LINE ( 'NONE', #9044, #1817 ) ;
#7433 = ORIENTED_EDGE ( 'NONE', *, *, #247, .F. ) ;
#7434 = CIRCLE ( 'NONE', #8155, 2.999999999999999112 ) ;
#7435 = DIRECTION ( 'NONE',  ( 0.000000000000000000, 0.000000000000000000, 1.000000000000000000 ) ) ;
#7436 = ORIENTED_EDGE ( 'NONE', *, *, #3055, .F. ) ;
#7437 = AXIS2_PLACEMENT_3D ( 'NONE', #4071, #9245, #922 ) ;
#7438 = DIRECTION ( 'NONE',  ( 0.000000000000000000, 1.000000000000000000, 0.000000000000000000 ) ) ;
#7439 = DIRECTION ( 'NONE',  ( 0.000000000000000000, 0.000000000000000000, 1.000000000000000000 ) ) ;
#7440 = APPLICATION_CONTEXT ( 'automotive_design' ) ;
#7441 = DIRECTION ( 'NONE',  ( 0.000000000000000000, 0.000000000000000000, 1.000000000000000000 ) ) ;
#7442 = ORIENTED_EDGE ( 'NONE', *, *, #3317, .T. ) ;
#7443 = CARTESIAN_POINT ( 'NONE',  ( -1.500000000000001332, 0.000000000000000000, 0.000000000000000000 ) ) ;
#7444 = CARTESIAN_POINT ( 'NONE',  ( -10.19839929293505776, 2.531249999044085097, -24.62111388750000174 ) ) ;
#7445 = AXIS2_PLACEMENT_3D ( 'NONE', #3662, #4273, #9342 ) ;
#7446 = EDGE_CURVE ( 'NONE', #399, #8513, #4086, .T. ) ;
#7447 = VERTEX_POINT ( 'NONE', #1532 ) ;
#7448 = EDGE_LOOP ( 'NONE', ( #6790, #7442, #10447, #7954 ) ) ;
#7449 =( BOUNDED_CURVE ( )  B_SPLINE_CURVE ( 2, ( #2738, #9495, #4489, #273, #3635, #5004, #9076, #10734, #10 ),
 .UNSPECIFIED., .F., .F. ) 
 B_SPLINE_CURVE_WITH_KNOTS ( ( 3, 2, 2, 2, 3 ),
 ( 0.5500000000000000444, 0.5749999999999999556, 0.5999999999999999778, 0.6250000000000000000, 0.6500000000000000222 ),
 .UNSPECIFIED. ) 
 CURVE ( )  GEOMETRIC_REPRESENTATION_ITEM ( )  RATIONAL_B_SPLINE_CURVE ( ( 1.000000000000000000, 0.9238795325112867385, 1.000000000000000000, 0.9238795325112867385, 1.000000000000000000, 0.9238795325112867385, 1.000000000000000000, 0.9238795325112867385, 1.000000000000000000 ) ) 
 REPRESENTATION_ITEM ( '' )  );
#7450 = CIRCLE ( 'NONE', #2687, 24.91176187412963117 ) ;
#7451 = EDGE_LOOP ( 'NONE', ( #10021, #393, #6578, #47 ) ) ;
#7452 = AXIS2_PLACEMENT_3D ( 'NONE', #8328, #8267, #3075 ) ;
#7453 = EDGE_CURVE ( 'NONE', #698, #5893, #2308, .T. ) ;
#7454 = CARTESIAN_POINT ( 'NONE',  ( -4.592425496802574367E-15, 5.362499998088169129, 25.00000000000000000 ) ) ;
#7455 = LINE ( 'NONE', #5592, #8286 ) ;
#7456 = VECTOR ( 'NONE', #3227, 1000.000000000000000 ) ;
#7457 = CARTESIAN_POINT ( 'NONE',  ( 10.19839929293505953, 2.406249999044085541, -24.62111388750000174 ) ) ;
#7458 = DIRECTION ( 'NONE',  ( 1.000000000000000000, 0.000000000000000000, 0.000000000000000000 ) ) ;
#7459 = ORIENTED_EDGE ( 'NONE', *, *, #2543, .T. ) ;
#7460 = DIRECTION ( 'NONE',  ( 0.000000000000000000, 1.000000000000000000, 0.000000000000000000 ) ) ;
#7461 = CARTESIAN_POINT ( 'NONE',  ( -10.35533905932736687, 1.924999998088168907, -25.00000000000000711 ) ) ;
#7462 = AXIS2_PLACEMENT_3D ( 'NONE', #147, #8478, #4233 ) ;
#7463 = CARTESIAN_POINT ( 'NONE',  ( 82.32050807568876394, 92.28203230275514102, 5.000000000000000000 ) ) ;
#7464 = DIRECTION ( 'NONE',  ( 0.000000000000000000, 0.000000000000000000, 1.000000000000000000 ) ) ;
#7465 = CIRCLE ( 'NONE', #7277, 5.000000000000005329 ) ;
#7466 = DIRECTION ( 'NONE',  ( 0.000000000000000000, 1.000000000000000000, 0.000000000000000000 ) ) ;
#7467 = EDGE_CURVE ( 'NONE', #9967, #57, #4522, .T. ) ;
#7468 = ADVANCED_FACE ( 'NONE', ( #4710 ), #8057, .T. ) ;
#7469 = AXIS2_PLACEMENT_3D ( 'NONE', #9257, #1702, #10154 ) ;
#7470 = ORIENTED_EDGE ( 'NONE', *, *, #3247, .T. ) ;
#7471 = ORIENTED_EDGE ( 'NONE', *, *, #10331, .T. ) ;
#7472 = AXIS2_PLACEMENT_3D ( 'NONE', #2123, #1251, #367 ) ;
#7473 = UNCERTAINTY_MEASURE_WITH_UNIT (LENGTH_MEASURE( 1.000000000000000082E-05 ), #2620, 'distance_accuracy_value', 'NONE');
#7474 = EDGE_CURVE ( 'NONE', #2098, #5999, #2568, .T. ) ;
#7475 = CARTESIAN_POINT ( 'NONE',  ( -17.67766952966369232, 5.237499998088169129, 17.67766952966368876 ) ) ;
#7476 = CARTESIAN_POINT ( 'NONE',  ( -24.62111388750000174, 0.6562499990440846531, -10.19839929293506131 ) ) ;
#7477 = DIRECTION ( 'NONE',  ( 0.9449111825230666062, -0.000000000000000000, -0.3273268353539928177 ) ) ;
#7478 = PLANE ( 'NONE',  #1073 ) ;
#7479 = CARTESIAN_POINT ( 'NONE',  ( 17.40975659021752620, 1.093749999044084653, 17.40975659021753330 ) ) ;
#7480 = DIRECTION ( 'NONE',  ( 0.000000000000000000, -1.000000000000000000, 0.000000000000000000 ) ) ;
#7481 = CARTESIAN_POINT ( 'NONE',  ( -10.19839929293507552, 2.906249999044085541, 24.62111388749999463 ) ) ;
#7482 = FACE_OUTER_BOUND ( 'NONE', #2394, .T. ) ;
#7483 = ORIENTED_EDGE ( 'NONE', *, *, #5389, .T. ) ;
#7484 = ORIENTED_EDGE ( 'NONE', *, *, #5050, .T. ) ;
#7485 = EDGE_LOOP ( 'NONE', ( #1710, #625, #9374, #934 ) ) ;
#7486 = EDGE_CURVE ( 'NONE', #5695, #6733, #6848, .T. ) ;
#7487 = VERTEX_POINT ( 'NONE', #6684 ) ;
#7488 = EDGE_CURVE ( 'NONE', #7766, #748, #3459, .T. ) ;
#7489 = DIRECTION ( 'NONE',  ( 0.000000000000000000, 0.000000000000000000, -1.000000000000000000 ) ) ;
#7490 = CARTESIAN_POINT ( 'NONE',  ( 0.000000000000000000, 5.000000000000000000, -25.00000000000000000 ) ) ;
#7491 = LINE ( 'NONE', #815, #4503 ) ;
#7492 = DIRECTION ( 'NONE',  ( 0.8660254037844327124, 0.000000000000000000, -0.5000000000000103251 ) ) ;
#7493 = CARTESIAN_POINT ( 'NONE',  ( 8.318560929346013211, 5.000000000000000000, 23.22693844957334619 ) ) ;
#7494 = EDGE_CURVE ( 'NONE', #2252, #8568, #10040, .T. ) ;
#7495 = ORIENTED_EDGE ( 'NONE', *, *, #8684, .F. ) ;
#7496 = ORIENTED_EDGE ( 'NONE', *, *, #7749, .T. ) ;
#7497 = DIRECTION ( 'NONE',  ( 0.000000000000000000, 0.000000000000000000, -1.000000000000000000 ) ) ;
#7498 = CARTESIAN_POINT ( 'NONE',  ( -1.500000000000000444, 83.00000000000000000, -1.500000000000000222 ) ) ;
#7499 = CARTESIAN_POINT ( 'NONE',  ( 0.000000000000000000, 88.00000000000001421, 0.000000000000000000 ) ) ;
#7500 = CYLINDRICAL_SURFACE ( 'NONE', #1441, 2.999999999999997335 ) ;
#7501 = ORIENTED_EDGE ( 'NONE', *, *, #6403, .F. ) ;
#7502 = CARTESIAN_POINT ( 'NONE',  ( 9.875000000000023093, 28.00000000000000000, 20.10400172474264835 ) ) ;
#7503 = APPLICATION_PROTOCOL_DEFINITION ( 'draft international standard', 'automotive_design', 1998, #9576 ) ;
#7504 = LINE ( 'NONE', #379, #7834 ) ;
#7505 = DIRECTION ( 'NONE',  ( 0.000000000000000000, 1.000000000000000000, 0.000000000000000000 ) ) ;
#7506 = CARTESIAN_POINT ( 'NONE',  ( -24.62111388750000884, 1.781249999044084875, 10.19839929293505421 ) ) ;
#7507 = ORIENTED_EDGE ( 'NONE', *, *, #5395, .T. ) ;
#7508 = EDGE_LOOP ( 'NONE', ( #1674, #1959, #3740, #3950 ) ) ;
#7509 = CARTESIAN_POINT ( 'NONE',  ( 17.40975659021752620, 4.268749999044084475, 17.40975659021753330 ) ) ;
#7510 = CARTESIAN_POINT ( 'NONE',  ( 0.000000000000000000, 5.000000000000000000, -25.00000000000000000 ) ) ;
#7511 = CARTESIAN_POINT ( 'NONE',  ( -24.62111388750000174, 0.7187499990440845421, -3.015216831376932151E-15 ) ) ;
#7512 = PRODUCT_DEFINITION ( 'UNKNOWN', '', #10401, #10793 ) ;
#7513 = DIRECTION ( 'NONE',  ( 1.000000000000000000, 0.000000000000000000, 0.000000000000000000 ) ) ;
#7514 = ORIENTED_EDGE ( 'NONE', *, *, #508, .T. ) ;
#7515 = DIRECTION ( 'NONE',  ( 0.000000000000000000, 0.5000000000000001110, 0.8660254037844387076 ) ) ;
#7516 = CARTESIAN_POINT ( 'NONE',  ( -9.874999999999777955, 28.00000000000000000, 17.10400172474279401 ) ) ;
#7517 = CARTESIAN_POINT ( 'NONE',  ( -7.276923788646840308, 28.00000000000000000, -18.60400172474260216 ) ) ;
#7518 = LINE ( 'NONE', #7569, #556 ) ;
#7519 = LINE ( 'NONE', #10898, #9335 ) ;
#7520 =( BOUNDED_CURVE ( )  B_SPLINE_CURVE ( 2, ( #4815, #8175, #5692, #9207, #9873, #1535, #657, #1652, #10766 ),
 .UNSPECIFIED., .F., .F. ) 
 B_SPLINE_CURVE_WITH_KNOTS ( ( 3, 2, 2, 2, 3 ),
 ( 0.2500000000000000000, 0.2750000000000000222, 0.3000000000000000444, 0.3250000000000000666, 0.3500000000000000333 ),
 .UNSPECIFIED. ) 
 CURVE ( )  GEOMETRIC_REPRESENTATION_ITEM ( )  RATIONAL_B_SPLINE_CURVE ( ( 1.000000000000000000, 0.9238795325112867385, 1.000000000000000000, 0.9238795325112867385, 1.000000000000000000, 0.9238795325112867385, 1.000000000000000000, 0.9238795325112865164, 1.000000000000000222 ) ) 
 REPRESENTATION_ITEM ( '' )  );
#7521 = CARTESIAN_POINT ( 'NONE',  ( 25.00000000000000000, 5.306249999044084120, 0.000000000000000000 ) ) ;
#7522 = EDGE_LOOP ( 'NONE', ( #8899, #9738, #5749, #2332 ) ) ;
#7523 = ORIENTED_EDGE ( 'NONE', *, *, #4589, .T. ) ;
#7524 = EDGE_CURVE ( 'NONE', #6576, #500, #5209, .T. ) ;
#7525 = ADVANCED_FACE ( 'NONE', ( #2411 ), #9984, .T. ) ;
#7526 = CARTESIAN_POINT ( 'NONE',  ( -17.40975659021753330, 2.018749999044084475, 17.40975659021752975 ) ) ;
#7527 = CARTESIAN_POINT ( 'NONE',  ( 24.62111388750000174, 1.281249999044084653, -10.19839929293505776 ) ) ;
#7528 = PRESENTATION_STYLE_ASSIGNMENT (( #1679 ) ) ;
#7529 = CARTESIAN_POINT ( 'NONE',  ( 3.924072712834459686, 19.03096903053429756, -5.796693311223905631 ) ) ;
#7530 = DIRECTION ( 'NONE',  ( 0.8660254037844433705, -0.000000000000000000, 0.4999999999999916733 ) ) ;
#7531 = CARTESIAN_POINT ( 'NONE',  ( 17.40975659021752620, 2.093749999044084653, 17.40975659021753330 ) ) ;
#7532 = DIRECTION ( 'NONE',  ( 1.000000000000000000, 0.000000000000000000, -0.000000000000000000 ) ) ;
#7533 = ADVANCED_FACE ( 'NONE', ( #10210 ), #6024, .F. ) ;
#7534 = ORIENTED_EDGE ( 'NONE', *, *, #5227, .T. ) ;
#7535 = VERTEX_POINT ( 'NONE', #43 ) ;
#7536 = EDGE_LOOP ( 'NONE', ( #8170, #8177, #7868, #6062 ) ) ;
#7537 = ORIENTED_EDGE ( 'NONE', *, *, #398, .F. ) ;
#7538 = CIRCLE ( 'NONE', #10003, 6.000000000000000888 ) ;
#7539 = EDGE_CURVE ( 'NONE', #1765, #457, #7609, .T. ) ;
#7540 = AXIS2_PLACEMENT_3D ( 'NONE', #10253, #6121, #7886 ) ;
#7541 = DIRECTION ( 'NONE',  ( 0.000000000000000000, 0.000000000000000000, 1.000000000000000000 ) ) ;
#7542 = DIRECTION ( 'NONE',  ( 0.000000000000000000, 0.000000000000000000, 1.000000000000000000 ) ) ;
#7543 = DIRECTION ( 'NONE',  ( -0.4999999999999888423, 0.000000000000000000, -0.8660254037844449249 ) ) ;
#7544 = CARTESIAN_POINT ( 'NONE',  ( -13.63990010960498367, -0.001000000000001000089, -4.874999999999872102 ) ) ;
#7545 = CARTESIAN_POINT ( 'NONE',  ( 24.33865891316265362, 5.000000000000000000, 5.618519342023028607 ) ) ;
#7546 = EDGE_CURVE ( 'NONE', #3125, #7292, #10882, .T. ) ;
#7547 = AXIS2_PLACEMENT_3D ( 'NONE', #1190, #7877, #4571 ) ;
#7548 = VECTOR ( 'NONE', #2322, 1000.000000000000000 ) ;
#7549 = EDGE_LOOP ( 'NONE', ( #1111, #6890, #8385, #2894 ) ) ;
#7550 = ORIENTED_EDGE ( 'NONE', *, *, #1322, .T. ) ;
#7551 = LINE ( 'NONE', #10090, #2998 ) ;
#7552 = CARTESIAN_POINT ( 'NONE',  ( -4.592425496802574367E-15, 0.7500000000000000000, 25.00000000000000000 ) ) ;
#7553 = ORIENTED_EDGE ( 'NONE', *, *, #9356, .F. ) ;
#7554 = CARTESIAN_POINT ( 'NONE',  ( -5.000000000000000000, 90.00000000000001421, -5.000000000000000000 ) ) ;
#7555 = CARTESIAN_POINT ( 'NONE',  ( 0.000000000000000000, 0.000000000000000000, 0.000000000000000000 ) ) ;
#7556 = CARTESIAN_POINT ( 'NONE',  ( -15.13990010960484867, 25.00000000000000000, 5.276923788646865177 ) ) ;
#7557 = VERTEX_POINT ( 'NONE', #7556 ) ;
#7558 = AXIS2_PLACEMENT_3D ( 'NONE', #3589, #3644, #10336 ) ;
#7559 = CARTESIAN_POINT ( 'NONE',  ( -17.40975659021753330, 3.843749999044085097, 17.40975659021752975 ) ) ;
#7560 = EDGE_LOOP ( 'NONE', ( #1925, #7263, #1721, #3814 ) ) ;
#7561 = FACE_OUTER_BOUND ( 'NONE', #7867, .T. ) ;
#7562 = CARTESIAN_POINT ( 'NONE',  ( -10.19839929293507552, 0.9062499990440844311, 24.62111388749999463 ) ) ;
#7563 = CARTESIAN_POINT ( 'NONE',  ( -12.47307621135344391, 25.00000000000000000, -15.60400172474256131 ) ) ;
#7564 = ORIENTED_EDGE ( 'NONE', *, *, #7073, .F. ) ;
#7565 = CARTESIAN_POINT ( 'NONE',  ( -10.35533905932737575, 3.312500000000000000, -25.00000000000000000 ) ) ;
#7566 =( LENGTH_UNIT ( ) NAMED_UNIT ( * ) SI_UNIT ( .MILLI., .METRE. ) );
#7567 = DIRECTION ( 'NONE',  ( -0.000000000000000000, 0.000000000000000000, -1.000000000000000000 ) ) ;
#7568 = DIRECTION ( 'NONE',  ( 0.000000000000000000, 0.000000000000000000, 1.000000000000000000 ) ) ;
#7569 = CARTESIAN_POINT ( 'NONE',  ( 18.60400172474268032, -0.001000000000001000089, 7.276923788646641356 ) ) ;
#7570 = CARTESIAN_POINT ( 'NONE',  ( 10.47307621135332667, 25.00000000000000000, 12.13990010960489840 ) ) ;
#7571 = AXIS2_PLACEMENT_3D ( 'NONE', #8801, #10620, #1239 ) ;
#7572 = VERTEX_POINT ( 'NONE', #6797 ) ;
#7573 = ORIENTED_EDGE ( 'NONE', *, *, #5408, .F. ) ;
#7574 = EDGE_LOOP ( 'NONE', ( #6815, #3810, #6269, #7621 ) ) ;
#7575 = ORIENTED_EDGE ( 'NONE', *, *, #436, .F. ) ;
#7576 = CARTESIAN_POINT ( 'NONE',  ( 24.62111388750000174, 2.393749999044084475, 0.000000000000000000 ) ) ;
#7577 = CARTESIAN_POINT ( 'NONE',  ( -10.19839929293507552, 1.081249999044084475, 24.62111388749999463 ) ) ;
#7578 = CARTESIAN_POINT ( 'NONE',  ( 24.62111388750000174, 2.281249999044085541, -10.19839929293505776 ) ) ;
#7579 = CARTESIAN_POINT ( 'NONE',  ( 2.262820851736500494, 10.00000000000000355, -9.633606397919622921 ) ) ;
#7580 = AXIS2_PLACEMENT_3D ( 'NONE', #10708, #8111, #4144 ) ;
#7581 = AXIS2_PLACEMENT_3D ( 'NONE', #7858, #8052, #6302 ) ;
#7582 = EDGE_LOOP ( 'NONE', ( #4485, #9213, #10875, #7495 ) ) ;
#7583 = DIRECTION ( 'NONE',  ( 0.2499999999999950318, 0.8660254037844380415, 0.4330127018922235171 ) ) ;
#7584 = CARTESIAN_POINT ( 'NONE',  ( 24.62111388750000174, 0.3062499990440845643, 0.000000000000000000 ) ) ;
#7585 = CARTESIAN_POINT ( 'NONE',  ( 67.97877056362573001, 89.28203230275514102, 5.000000000000000000 ) ) ;
#7586 = EDGE_LOOP ( 'NONE', ( #10867, #2720, #9197 ) ) ;
#7587 = ORIENTED_EDGE ( 'NONE', *, *, #5211, .F. ) ;
#7588 = EDGE_CURVE ( 'NONE', #5226, #9241, #8875, .T. ) ;
#7589 = ORIENTED_EDGE ( 'NONE', *, *, #5704, .T. ) ;
#7590 = ORIENTED_EDGE ( 'NONE', *, *, #9075, .T. ) ;
#7591 = VECTOR ( 'NONE', #2674, 1000.000000000000000 ) ;
#7592 = CIRCLE ( 'NONE', #2824, 25.00000000000000000 ) ;
#7593 = ORIENTED_EDGE ( 'NONE', *, *, #3909, .T. ) ;
#7594 = EDGE_CURVE ( 'NONE', #3717, #10548, #680, .T. ) ;
#7595 = CARTESIAN_POINT ( 'NONE',  ( 82.32050807568876394, 100.2820323027551268, 3.379762621896238883 ) ) ;
#7596 = PLANE ( 'NONE',  #5016 ) ;
#7597 = LINE ( 'NONE', #864, #10486 ) ;
#7598 = CARTESIAN_POINT ( 'NONE',  ( 0.000000000000000000, 5.000000000000000000, 0.000000000000000000 ) ) ;
#7599 = DIRECTION ( 'NONE',  ( 0.4330127018922191318, -0.8660254037844380415, 0.2500000000000026090 ) ) ;
#7600 = ADVANCED_FACE ( 'NONE', ( #5962, #3343 ), #9206, .T. ) ;
#7601 = ORIENTED_EDGE ( 'NONE', *, *, #7846, .F. ) ;
#7602 = ADVANCED_FACE ( 'NONE', ( #1650 ), #7645, .T. ) ;
#7603 = CARTESIAN_POINT ( 'NONE',  ( 0.5000000000000000000, 10.00000000000000355, -6.982120021884467675 ) ) ;
#7604 = FACE_OUTER_BOUND ( 'NONE', #9552, .T. ) ;
#7605 = VECTOR ( 'NONE', #8362, 1000.000000000000000 ) ;
#7606 = CARTESIAN_POINT ( 'NONE',  ( 0.000000000000000000, 10.00000000000000355, 0.000000000000000000 ) ) ;
#7607 = ORIENTED_EDGE ( 'NONE', *, *, #10696, .F. ) ;
#7608 = PLANE ( 'NONE',  #7078 ) ;
#7609 = LINE ( 'NONE', #8551, #9755 ) ;
#7610 = LINE ( 'NONE', #10333, #7273 ) ;
#7611 = DIRECTION ( 'NONE',  ( 0.000000000000000000, 1.000000000000000000, 0.000000000000000000 ) ) ;
#7612 = SHAPE_REPRESENTATION ( 'angular contact ball bearing_68_iso_ISO 15 ABB - 1710 - 20,SI,NC,20_68', ( #7040 ), #4727 ) ;
#7613 = ORIENTED_EDGE ( 'NONE', *, *, #1144, .T. ) ;
#7614 = AXIS2_PLACEMENT_3D ( 'NONE', #6592, #9171, #617 ) ;
#7615 = ADVANCED_FACE ( 'NONE', ( #6739 ), #2017, .T. ) ;
#7616 = AXIS2_PLACEMENT_3D ( 'NONE', #5030, #8378, #4187 ) ;
#7617 = FACE_OUTER_BOUND ( 'NONE', #4854, .T. ) ;
#7618 = CARTESIAN_POINT ( 'NONE',  ( -1.400000000000001910, 0.000000000000000000, 0.000000000000000000 ) ) ;
#7619 = CARTESIAN_POINT ( 'NONE',  ( 0.000000000000000000, -58.00000000000000000, 24.91176187412963117 ) ) ;
#7620 = CARTESIAN_POINT ( 'NONE',  ( 0.000000000000000000, 85.00000000000000000, 0.000000000000000000 ) ) ;
#7621 = ORIENTED_EDGE ( 'NONE', *, *, #10512, .F. ) ;
#7622 = CARTESIAN_POINT ( 'NONE',  ( 12.47307621135333200, -0.001000000000001000089, 15.60400172474264835 ) ) ;
#7623 = VECTOR ( 'NONE', #6502, 1000.000000000000000 ) ;
#7624 = DIRECTION ( 'NONE',  ( -0.000000000000000000, 1.000000000000000000, -0.000000000000000000 ) ) ;
#7625 = VECTOR ( 'NONE', #6548, 999.9999999999998863 ) ;
#7626 = CARTESIAN_POINT ( 'NONE',  ( 28.09696521099633060, 102.8977774788672264, 5.000000000000000000 ) ) ;
#7627 = LINE ( 'NONE', #1220, #8852 ) ;
#7628 = DIRECTION ( 'NONE',  ( -0.000000000000000000, -1.000000000000000000, -0.000000000000000000 ) ) ;
#7629 = CIRCLE ( 'NONE', #7437, 5.000000000000000888 ) ;
#7630 = VECTOR ( 'NONE', #9904, 1000.000000000000000 ) ;
#7631 = ORIENTED_EDGE ( 'NONE', *, *, #4313, .T. ) ;
#7632 = ORIENTED_EDGE ( 'NONE', *, *, #1478, .F. ) ;
#7633 = VECTOR ( 'NONE', #6116, 1000.000000000000000 ) ;
#7634 = ORIENTED_EDGE ( 'NONE', *, *, #1075, .T. ) ;
#7635 = CARTESIAN_POINT ( 'NONE',  ( 0.000000000000000000, 10.00000000000000355, 0.000000000000000000 ) ) ;
#7636 = CARTESIAN_POINT ( 'NONE',  ( 17.40975659021752975, 4.518749999044085364, -17.40975659021752975 ) ) ;
#7637 = CARTESIAN_POINT ( 'NONE',  ( 0.1920286436967143240, 1.533495552763497570E-16, 5.525000000000006573 ) ) ;
#7638 = CARTESIAN_POINT ( 'NONE',  ( 17.40975659021752620, 2.268749999044084475, 17.40975659021753330 ) ) ;
#7639 = CIRCLE ( 'NONE', #4831, 6.999999999999997335 ) ;
#7640 = CARTESIAN_POINT ( 'NONE',  ( -24.62111388750000174, 3.718749999044084653, -3.015216831376932151E-15 ) ) ;
#7641 = AXIS2_PLACEMENT_3D ( 'NONE', #8374, #816, #5899 ) ;
#7642 = CARTESIAN_POINT ( 'NONE',  ( 68.37372805638788975, 92.28203230275514102, -5.000000000000000000 ) ) ;
#7643 = CARTESIAN_POINT ( 'NONE',  ( 0.000000000000000000, 88.00000000000001421, -30.00000000000000000 ) ) ;
#7644 = DIRECTION ( 'NONE',  ( 0.000000000000000000, 2.775557561562888270E-17, 1.000000000000000000 ) ) ;
#7645 = CONICAL_SURFACE ( 'NONE', #10296, 1.610000000000003872, 1.047197551196600518 ) ;
#7646 = CARTESIAN_POINT ( 'NONE',  ( -24.62111388750000174, 4.718749999044084653, -3.015216831376932151E-15 ) ) ;
#7647 = CARTESIAN_POINT ( 'NONE',  ( -17.67766952966368876, 2.987499998088169129, -17.67766952966369232 ) ) ;
#7648 = ORIENTED_EDGE ( 'NONE', *, *, #3755, .F. ) ;
#7649 = EDGE_LOOP ( 'NONE', ( #6888, #8272, #5116 ) ) ;
#7650 = AXIS2_PLACEMENT_3D ( 'NONE', #6836, #6007, #6899 ) ;
#7651 = ORIENTED_EDGE ( 'NONE', *, *, #5590, .T. ) ;
#7652 = CARTESIAN_POINT ( 'NONE',  ( 0.000000000000000000, 82.00000000000000000, 0.000000000000000000 ) ) ;
#7653 = CIRCLE ( 'NONE', #6428, 4.500000000000000888 ) ;
#7654 = DIRECTION ( 'NONE',  ( 0.000000000000000000, -2.775557561562888270E-17, -1.000000000000000000 ) ) ;
#7655 = ORIENTED_EDGE ( 'NONE', *, *, #4796, .T. ) ;
#7656 = EDGE_CURVE ( 'NONE', #500, #10484, #1641, .T. ) ;
#7657 = CARTESIAN_POINT ( 'NONE',  ( 1.530808498934191521E-15, 2.250000000000000444, -25.00000000000000000 ) ) ;
#7658 = CARTESIAN_POINT ( 'NONE',  ( 6.994037468151970138, 19.34316356887877220, 0.3335819196118934293 ) ) ;
#7659 = DIRECTION ( 'NONE',  ( 0.5000000000000073275, 0.000000000000000000, 0.8660254037844343777 ) ) ;
#7660 = LINE ( 'NONE', #7936, #1083 ) ;
#7661 = CARTESIAN_POINT ( 'NONE',  ( 23.96357173135144691, 5.000000000000001776, 6.992167731761885996 ) ) ;
#7662 = ORIENTED_EDGE ( 'NONE', *, *, #9566, .F. ) ;
#7663 = EDGE_CURVE ( 'NONE', #5308, #7827, #1589, .T. ) ;
#7664 = ORIENTED_EDGE ( 'NONE', *, *, #9778, .T. ) ;
#7665 = CARTESIAN_POINT ( 'NONE',  ( -4.592425496802574367E-15, 4.750000000000000000, 25.00000000000000000 ) ) ;
#7666 = DIRECTION ( 'NONE',  ( 0.7559289460184543952, -0.000000000000000000, 0.6546536707079771977 ) ) ;
#7667 = CARTESIAN_POINT ( 'NONE',  ( 10.35533905932742016, 5.424999998088169129, 24.99999999999996447 ) ) ;
#7668 = EDGE_CURVE ( 'NONE', #346, #3961, #7504, .T. ) ;
#7669 = CARTESIAN_POINT ( 'NONE',  ( 0.000000000000000000, 10.00000000000000355, 0.000000000000000000 ) ) ;
#7670 = EDGE_CURVE ( 'NONE', #3699, #716, #3393, .T. ) ;
#7671 = CARTESIAN_POINT ( 'NONE',  ( -1.500000000000001332, 0.000000000000000000, 0.000000000000000000 ) ) ;
#7672 = ADVANCED_FACE ( 'NONE', ( #4597 ), #10490, .T. ) ;
#7673 = CARTESIAN_POINT ( 'NONE',  ( 0.000000000000000000, 0.000000000000000000, 0.000000000000000000 ) ) ;
#7674 = CARTESIAN_POINT ( 'NONE',  ( 0.000000000000000000, 10.00000000000000355, 0.000000000000000000 ) ) ;
#7675 = CARTESIAN_POINT ( 'NONE',  ( -24.62111388750000174, 3.656249999044084653, -10.19839929293506131 ) ) ;
#7676 = ADVANCED_FACE ( 'NONE', ( #1995 ), #5460, .F. ) ;
#7677 = CARTESIAN_POINT ( 'NONE',  ( -24.62111388750000884, 2.956249999044084475, 10.19839929293505421 ) ) ;
#7678 = CARTESIAN_POINT ( 'NONE',  ( 10.00000000000000000, 90.00000000000001421, 5.000000000000000000 ) ) ;
#7679 = FACE_OUTER_BOUND ( 'NONE', #10063, .T. ) ;
#7680 = CARTESIAN_POINT ( 'NONE',  ( 0.000000000000000000, 20.00000000000000355, -2.000000000000000000 ) ) ;
#7681 = ORIENTED_EDGE ( 'NONE', *, *, #567, .F. ) ;
#7682 = EDGE_CURVE ( 'NONE', #6575, #39, #9502, .T. ) ;
#7683 = LINE ( 'NONE', #1776, #9333 ) ;
#7684 = DIRECTION ( 'NONE',  ( 0.000000000000000000, 1.000000000000000000, 0.000000000000000000 ) ) ;
#7685 = SHAPE_REPRESENTATION ( 'lid', ( #7040 ), #7026 ) ;
#7686 = DIRECTION ( 'NONE',  ( -0.000000000000000000, -1.000000000000000000, -0.000000000000000000 ) ) ;
#7687 = CARTESIAN_POINT ( 'NONE',  ( -17.67766952966368876, 1.987499998088169129, -17.67766952966369232 ) ) ;
#7688 = CARTESIAN_POINT ( 'NONE',  ( -7.276923788646840308, 25.00000000000000000, -18.60400172474260216 ) ) ;
#7689 = CARTESIAN_POINT ( 'NONE',  ( 1.530808498934191521E-15, 4.250000000000000000, -25.00000000000000000 ) ) ;
#7690 = ADVANCED_FACE ( 'NONE', ( #5417, #1113 ), #1171, .F. ) ;
#7691 = ORIENTED_EDGE ( 'NONE', *, *, #2012, .T. ) ;
#7692 = VERTEX_POINT ( 'NONE', #8775 ) ;
#7693 = ORIENTED_EDGE ( 'NONE', *, *, #792, .F. ) ;
#7694 = ORIENTED_EDGE ( 'NONE', *, *, #8689, .T. ) ;
#7695 = DIRECTION ( 'NONE',  ( 1.000000000000000000, 0.000000000000000000, -2.168404344971010347E-16 ) ) ;
#7696 = CARTESIAN_POINT ( 'NONE',  ( -24.62111388750000884, 4.956249999044084475, 10.19839929293505421 ) ) ;
#7697 = CARTESIAN_POINT ( 'NONE',  ( -24.62111388750000174, 0.8312499990440845865, -10.19839929293506131 ) ) ;
#7698 = CARTESIAN_POINT ( 'NONE',  ( -17.40975659021752975, 2.768749999044084475, -17.40975659021752975 ) ) ;
#7699 = CARTESIAN_POINT ( 'NONE',  ( -4.522825247065398226E-15, 4.968749999044083765, 24.62111388750000174 ) ) ;
#7700 = DIRECTION ( 'NONE',  ( 0.000000000000000000, 1.000000000000000000, 0.000000000000000000 ) ) ;
#7701 = DIRECTION ( 'NONE',  ( -0.4330127018922226290, -0.8660254037844380415, 0.2499999999999965028 ) ) ;
#7702 = FACE_BOUND ( 'NONE', #1783, .T. ) ;
#7703 = DIRECTION ( 'NONE',  ( -0.000000000000000000, -1.000000000000000000, -0.000000000000000000 ) ) ;
#7704 = DIRECTION ( 'NONE',  ( 0.000000000000000000, -2.775557561562888270E-17, -1.000000000000000000 ) ) ;
#7705 = ORIENTED_EDGE ( 'NONE', *, *, #2807, .F. ) ;
#7706 = ORIENTED_EDGE ( 'NONE', *, *, #3048, .F. ) ;
#7707 = VERTEX_POINT ( 'NONE', #8670 ) ;
#7708 = ORIENTED_EDGE ( 'NONE', *, *, #8885, .T. ) ;
#7709 = EDGE_LOOP ( 'NONE', ( #9083, #10902, #8531, #10346, #902 ) ) ;
#7710 = CARTESIAN_POINT ( 'NONE',  ( 18.60400172474263414, -0.001000000000001000089, -7.276923788646775471 ) ) ;
#7711 =( GEOMETRIC_REPRESENTATION_CONTEXT ( 3 ) GLOBAL_UNCERTAINTY_ASSIGNED_CONTEXT ( ( #9897 ) ) GLOBAL_UNIT_ASSIGNED_CONTEXT ( ( #7566, #3186, #667 ) ) REPRESENTATION_CONTEXT ( 'NONE', 'WORKASPACE' ) );
#7712 = CARTESIAN_POINT ( 'NONE',  ( 2.500000000000000444, -1.000000000000003331, 0.5773502691896272854 ) ) ;
#7713 = VERTEX_POINT ( 'NONE', #4548 ) ;
#7714 = CARTESIAN_POINT ( 'NONE',  ( 3.355508642977448552, 19.66631150450993104, 6.145599950363612507 ) ) ;
#7715 = DIRECTION ( 'NONE',  ( 0.000000000000000000, 1.000000000000000000, 0.000000000000000000 ) ) ;
#7716 = DIRECTION ( 'NONE',  ( 0.000000000000000000, -1.000000000000000000, 0.000000000000000000 ) ) ;
#7717 = DIRECTION ( 'NONE',  ( -0.000000000000000000, -1.000000000000000000, -0.000000000000000000 ) ) ;
#7718 = DIRECTION ( 'NONE',  ( 0.000000000000000000, 0.000000000000000000, 1.000000000000000000 ) ) ;
#7719 = ORIENTED_EDGE ( 'NONE', *, *, #5262, .F. ) ;
#7720 = VECTOR ( 'NONE', #1991, 1000.000000000000000 ) ;
#7721 = VERTEX_POINT ( 'NONE', #9611 ) ;
#7722 = CLOSED_SHELL ( 'NONE', ( #3550, #2993, #10081, #7533, #8640, #602, #7142, #774, #105, #10275, #2888, #3542, #6415, #5574, #4921, #3139, #5724, #1377, #6874, #6267, #8600, #6610, #10562, #5126, #7135, #2880, #9291, #3756 ) ) ;
#7723 =( NAMED_UNIT ( * ) SI_UNIT ( $, .STERADIAN. ) SOLID_ANGLE_UNIT ( ) );
#7724 = CARTESIAN_POINT ( 'NONE',  ( 1.530808498934191521E-15, 4.250000000000000000, -25.00000000000000000 ) ) ;
#7725 = CARTESIAN_POINT ( 'NONE',  ( 1.507608415688466075E-15, 4.643749999044084475, -24.62111388750000174 ) ) ;
#7726 = DIRECTION ( 'NONE',  ( -0.5000000000000009992, 0.8660254037844380415, -1.745740669421570228E-15 ) ) ;
#7727 = DIRECTION ( 'NONE',  ( 0.8660254037844399289, 0.000000000000000000, 0.4999999999999978351 ) ) ;
#7728 = STYLED_ITEM ( 'NONE', ( #2163 ), #715 ) ;
#7729 = CARTESIAN_POINT ( 'NONE',  ( 0.000000000000000000, 85.00000000000000000, 0.000000000000000000 ) ) ;
#7730 = DIRECTION ( 'NONE',  ( 0.000000000000000000, -1.000000000000000000, 0.000000000000000000 ) ) ;
#7731 = AXIS2_PLACEMENT_3D ( 'NONE', #4772, #2109, #10619 ) ;
#7732 = EDGE_CURVE ( 'NONE', #2380, #956, #2697, .T. ) ;
#7733 = EDGE_CURVE ( 'NONE', #514, #2380, #8730, .T. ) ;
#7734 = EDGE_CURVE ( 'NONE', #10248, #1133, #9063, .T. ) ;
#7735 = CARTESIAN_POINT ( 'NONE',  ( -24.62111388750000884, 0.9562499990440846975, 10.19839929293505421 ) ) ;
#7736 = LINE ( 'NONE', #2471, #534 ) ;
#7737 = VECTOR ( 'NONE', #9518, 1000.000000000000000 ) ;
#7738 = CARTESIAN_POINT ( 'NONE',  ( -17.40975659021753330, 4.843749999044083765, 17.40975659021752975 ) ) ;
#7739 = CARTESIAN_POINT ( 'NONE',  ( 10.19839929293505953, 1.581249999044084475, -24.62111388750000174 ) ) ;
#7740 = ORIENTED_EDGE ( 'NONE', *, *, #10789, .F. ) ;
#7741 = CARTESIAN_POINT ( 'NONE',  ( -10.35533905932739174, 1.299999998088168907, 24.99999999999999289 ) ) ;
#7742 = EDGE_CURVE ( 'NONE', #3157, #6934, #1935, .T. ) ;
#7743 = LINE ( 'NONE', #2579, #2345 ) ;
#7744 = CARTESIAN_POINT ( 'NONE',  ( 7.276923788646576519, 25.00000000000000000, -18.60400172474270519 ) ) ;
#7745 = CARTESIAN_POINT ( 'NONE',  ( 25.00000000000000000, 2.674999998088169129, -10.35533905932737753 ) ) ;
#7746 = CARTESIAN_POINT ( 'NONE',  ( 82.32050807568876394, 99.93473594742127375, 5.349378127920655146 ) ) ;
#7747 = CARTESIAN_POINT ( 'NONE',  ( -10.35533905932737575, 3.312500000000000000, -25.00000000000000000 ) ) ;
#7748 = ORIENTED_EDGE ( 'NONE', *, *, #10583, .F. ) ;
#7749 = EDGE_CURVE ( 'NONE', #10609, #2933, #3747, .T. ) ;
#7750 = ORIENTED_EDGE ( 'NONE', *, *, #4788, .F. ) ;
#7751 = DIRECTION ( 'NONE',  ( 0.000000000000000000, 0.000000000000000000, 1.000000000000000000 ) ) ;
#7752 = CARTESIAN_POINT ( 'NONE',  ( -17.40975659021752975, 2.768749999044084475, -17.40975659021752975 ) ) ;
#7753 = CARTESIAN_POINT ( 'NONE',  ( -24.62111388750000884, 0.9562499990440846975, 10.19839929293505421 ) ) ;
#7754 = CARTESIAN_POINT ( 'NONE',  ( 25.00000000000000000, 4.674999998088169129, -10.35533905932737753 ) ) ;
#7755 = CARTESIAN_POINT ( 'NONE',  ( 24.62111388750000174, 3.281249999044085097, -10.19839929293505776 ) ) ;
#7756 = CARTESIAN_POINT ( 'NONE',  ( -10.35533905932739174, 3.299999998088169129, 24.99999999999999289 ) ) ;
#7757 = EDGE_CURVE ( 'NONE', #9309, #7572, #2743, .T. ) ;
#7758 = ORIENTED_EDGE ( 'NONE', *, *, #3199, .F. ) ;
#7759 = CARTESIAN_POINT ( 'NONE',  ( 67.32050807568876394, 92.28203230275514102, 5.000000000000000000 ) ) ;
#7760 = CARTESIAN_POINT ( 'NONE',  ( 6.296693311223917178, 19.03096903053430822, -3.058047309049999996 ) ) ;
#7761 = DIRECTION ( 'NONE',  ( -1.000000000000000000, 0.000000000000000000, 0.000000000000000000 ) ) ;
#7762 = CARTESIAN_POINT ( 'NONE',  ( 24.99999999999999289, 4.937500000000001776, 10.35533905932739529 ) ) ;
#7763 = CARTESIAN_POINT ( 'NONE',  ( 24.62111388750000174, 5.218749999044084653, 0.000000000000000000 ) ) ;
#7764 = CARTESIAN_POINT ( 'NONE',  ( -4.592425496802574367E-15, 2.750000000000000000, 25.00000000000000000 ) ) ;
#7765 = AXIS2_PLACEMENT_3D ( 'NONE', #4032, #6569, #10763 ) ;
#7766 = VERTEX_POINT ( 'NONE', #2899 ) ;
#7767 = VERTEX_POINT ( 'NONE', #6298 ) ;
#7768 = ORIENTED_EDGE ( 'NONE', *, *, #4019, .F. ) ;
#7769 = PRODUCT_DEFINITION_SHAPE ( 'NONE', 'NONE',  #10146 ) ;
#7770 = CARTESIAN_POINT ( 'NONE',  ( -5.446152422706653340, 10.00000000000000355, 2.566987298107729742 ) ) ;
#7771 = AXIS2_PLACEMENT_3D ( 'NONE', #2796, #4645, #10435 ) ;
#7772 = VECTOR ( 'NONE', #4048, 1000.000000000000000 ) ;
#7773 = ADVANCED_FACE ( 'NONE', ( #3584 ), #6136, .F. ) ;
#7774 = CARTESIAN_POINT ( 'NONE',  ( -10.47307621135341904, -0.001000000000001000089, -12.13990010960482557 ) ) ;
#7775 = CARTESIAN_POINT ( 'NONE',  ( -20.63749999999999929, 0.000000000000000000, 0.000000000000000000 ) ) ;
#7776 = CARTESIAN_POINT ( 'NONE',  ( -0.5000000000000000000, 19.03096903053430822, -6.982120021884467675 ) ) ;
#7777 = DIRECTION ( 'NONE',  ( 0.000000000000000000, -1.000000000000000000, 0.000000000000000000 ) ) ;
#7778 = CARTESIAN_POINT ( 'NONE',  ( -5.000000000000000000, 90.00000000000001421, 5.000000000000000000 ) ) ;
#7779 = CARTESIAN_POINT ( 'NONE',  ( -15.13990010960496235, -0.001000000000001000089, -5.276923788646544544 ) ) ;
#7780 = FACE_OUTER_BOUND ( 'NONE', #6006, .T. ) ;
#7781 = VECTOR ( 'NONE', #3458, 999.9999999999998863 ) ;
#7782 = AXIS2_PLACEMENT_3D ( 'NONE', #2372, #8223, #9780 ) ;
#7783 = ORIENTED_EDGE ( 'NONE', *, *, #6453, .F. ) ;
#7784 = VERTEX_POINT ( 'NONE', #3520 ) ;
#7785 = AXIS2_PLACEMENT_3D ( 'NONE', #4738, #2230, #1403 ) ;
#7786 = PLANE ( 'NONE',  #10749 ) ;
#7787 = STYLED_ITEM ( 'NONE', ( #10600 ), #3360 ) ;
#7788 = CARTESIAN_POINT ( 'NONE',  ( -17.40975659021752975, 4.768749999044084475, -17.40975659021752975 ) ) ;
#7789 = CARTESIAN_POINT ( 'NONE',  ( -1.500000000000001332, 1.047786282324290395E-15, 6.975000000000000533 ) ) ;
#7790 = SHAPE_DEFINITION_REPRESENTATION ( #9332, #5021 ) ;
#7791 = DIRECTION ( 'NONE',  ( -1.000000000000000000, 0.000000000000000000, -7.228014483236695816E-17 ) ) ;
#7792 = DIRECTION ( 'NONE',  ( 0.000000000000000000, -0.000000000000000000, 1.000000000000000000 ) ) ;
#7793 = CARTESIAN_POINT ( 'NONE',  ( 67.32050807568876394, 89.28203230275514102, 5.000000000000000000 ) ) ;
#7794 = ORIENTED_EDGE ( 'NONE', *, *, #7314, .F. ) ;
#7795 = VECTOR ( 'NONE', #3958, 1000.000000000000000 ) ;
#7796 = CARTESIAN_POINT ( 'NONE',  ( -17.40975659021752975, 1.768749999044084475, -17.40975659021752975 ) ) ;
#7797 = DIRECTION ( 'NONE',  ( -0.5000000000000005551, 0.8660254037844383745, 0.000000000000000000 ) ) ;
#7798 = CARTESIAN_POINT ( 'NONE',  ( 1.499999999999999556, 88.00000000000001421, -1.500000000000000222 ) ) ;
#7799 = CARTESIAN_POINT ( 'NONE',  ( 0.000000000000000000, 82.00000000000000000, 6.000000000000000888 ) ) ;
#7800 = EDGE_LOOP ( 'NONE', ( #5099, #6519, #4851, #1183 ) ) ;
#7801 = CARTESIAN_POINT ( 'NONE',  ( -17.67766952966369232, 1.237499998088169129, 17.67766952966368876 ) ) ;
#7802 = DIRECTION ( 'NONE',  ( 0.000000000000000000, 0.000000000000000000, 1.000000000000000000 ) ) ;
#7803 = CARTESIAN_POINT ( 'NONE',  ( 17.40975659021752975, 0.3437499990440845421, -17.40975659021752975 ) ) ;
#7804 = EDGE_CURVE ( 'NONE', #7692, #7375, #1055, .T. ) ;
#7805 = PLANE ( 'NONE',  #5449 ) ;
#7806 = AXIS2_PLACEMENT_3D ( 'NONE', #9735, #5550, #7464 ) ;
#7807 = ORIENTED_EDGE ( 'NONE', *, *, #8198, .T. ) ;
#7808 = AXIS2_PLACEMENT_3D ( 'NONE', #5216, #7458, #5803 ) ;
#7809 = ORIENTED_EDGE ( 'NONE', *, *, #5771, .F. ) ;
#7810 = EDGE_CURVE ( 'NONE', #10901, #5101, #7847, .T. ) ;
#7811 = LINE ( 'NONE', #4389, #8617 ) ;
#7812 = CARTESIAN_POINT ( 'NONE',  ( -4.522825247065398226E-15, 5.143749999044084475, 24.62111388750000174 ) ) ;
#7813 = AXIS2_PLACEMENT_3D ( 'NONE', #6408, #536, #1521 ) ;
#7814 = CARTESIAN_POINT ( 'NONE',  ( 0.000000000000000000, 82.00000000000000000, 0.000000000000000000 ) ) ;
#7815 = CARTESIAN_POINT ( 'NONE',  ( -17.67766952966368876, 2.987499998088169129, -17.67766952966369232 ) ) ;
#7816 = CARTESIAN_POINT ( 'NONE',  ( -10.19839929293507552, 4.906249999044083765, 24.62111388749999463 ) ) ;
#7817 = CARTESIAN_POINT ( 'NONE',  ( 1.530808498934191521E-15, 2.862499998088169573, -25.00000000000000000 ) ) ;
#7818 = ADVANCED_FACE ( 'NONE', ( #4427 ), #7024, .F. ) ;
#7819 = CARTESIAN_POINT ( 'NONE',  ( 3.500000000000004885, 20.00000000000000355, -6.062177826491062405 ) ) ;
#7820 = CARTESIAN_POINT ( 'NONE',  ( 0.000000000000000000, 25.00000000000000000, 0.000000000000000000 ) ) ;
#7821 = CARTESIAN_POINT ( 'NONE',  ( 0.000000000000000000, 85.00000000000000000, -25.00000000000000000 ) ) ;
#7822 = VECTOR ( 'NONE', #2254, 1000.000000000000000 ) ;
#7823 = CARTESIAN_POINT ( 'NONE',  ( 1.530808498934191521E-15, 4.862499998088169129, -25.00000000000000000 ) ) ;
#7824 = CARTESIAN_POINT ( 'NONE',  ( -25.00000000000000000, 0.5000000000000000000, -3.061616997868383043E-15 ) ) ;
#7825 = LINE ( 'NONE', #3556, #6582 ) ;
#7826 = CIRCLE ( 'NONE', #9922, 0.7499999999999997780 ) ;
#7827 = VERTEX_POINT ( 'NONE', #1519 ) ;
#7828 = EDGE_CURVE ( 'NONE', #2551, #6450, #8723, .T. ) ;
#7829 =( BOUNDED_CURVE ( )  B_SPLINE_CURVE ( 3, ( #7529, #78, #9959, #5762 ),
 .UNSPECIFIED., .F., .F. ) 
 B_SPLINE_CURVE_WITH_KNOTS ( ( 4, 4 ),
 ( 3.927175151554406884, 3.998664601439927857 ),
 .UNSPECIFIED. ) 
 CURVE ( )  GEOMETRIC_REPRESENTATION_ITEM ( )  RATIONAL_B_SPLINE_CURVE ( ( 1.000000000000000000, 0.9995741502243209453, 0.9995741502243209453, 1.000000000000000000 ) ) 
 REPRESENTATION_ITEM ( '' )  );
#7830 = VERTEX_POINT ( 'NONE', #6349 ) ;
#7831 = AXIS2_PLACEMENT_3D ( 'NONE', #7164, #1250, #4689 ) ;
#7832 = FACE_OUTER_BOUND ( 'NONE', #2103, .T. ) ;
#7833 = AXIS2_PLACEMENT_3D ( 'NONE', #535, #4748, #9974 ) ;
#7834 = VECTOR ( 'NONE', #4496, 1000.000000000000000 ) ;
#7835 = DIRECTION ( 'NONE',  ( -0.000000000000000000, 1.000000000000000000, -0.000000000000000000 ) ) ;
#7836 = LINE ( 'NONE', #423, #2705 ) ;
#7837 = DIRECTION ( 'NONE',  ( 0.000000000000000000, 0.000000000000000000, 1.000000000000000000 ) ) ;
#7838 = DIRECTION ( 'NONE',  ( 0.000000000000000000, 0.000000000000000000, -1.000000000000000000 ) ) ;
#7839 = CARTESIAN_POINT ( 'NONE',  ( -17.10400172474254532, -0.001000000000001000089, 9.875000000000202505 ) ) ;
#7840 = FACE_OUTER_BOUND ( 'NONE', #4949, .T. ) ;
#7841 = AXIS2_PLACEMENT_3D ( 'NONE', #8653, #9600, #2034 ) ;
#7842 = CARTESIAN_POINT ( 'NONE',  ( -7.875000000000116351, 28.00000000000000000, -10.63990010960484334 ) ) ;
#7843 = EDGE_CURVE ( 'NONE', #3931, #10673, #2295, .T. ) ;
#7844 = ORIENTED_EDGE ( 'NONE', *, *, #6280, .T. ) ;
#7845 = VERTEX_POINT ( 'NONE', #10697 ) ;
#7846 = EDGE_CURVE ( 'NONE', #5377, #1334, #1651, .T. ) ;
#7847 = CIRCLE ( 'NONE', #9939, 6.999999999999997335 ) ;
#7848 = ORIENTED_EDGE ( 'NONE', *, *, #6201, .T. ) ;
#7849 = CYLINDRICAL_SURFACE ( 'NONE', #4629, 2.999999999999997335 ) ;
#7850 = LINE ( 'NONE', #1931, #7720 ) ;
#7851 = CARTESIAN_POINT ( 'NONE',  ( 10.19839929293505953, 1.581249999044084475, -24.62111388750000174 ) ) ;
#7852 = FACE_OUTER_BOUND ( 'NONE', #3346, .T. ) ;
#7853 = PRODUCT_CONTEXT ( 'NONE', #6337, 'mechanical' ) ;
#7854 = CARTESIAN_POINT ( 'NONE',  ( 2.857142857142858983, 10.00000000000000355, 9.474358296526935064 ) ) ;
#7855 = DIRECTION ( 'NONE',  ( -0.000000000000000000, -1.000000000000000000, -0.000000000000000000 ) ) ;
#7856 = LINE ( 'NONE', #4498, #4577 ) ;
#7857 = EDGE_CURVE ( 'NONE', #1860, #5496, #1315, .T. ) ;
#7858 = CARTESIAN_POINT ( 'NONE',  ( -2.999999999999996447, -0.001000000000001000089, 19.75000000000000000 ) ) ;
#7859 = CARTESIAN_POINT ( 'NONE',  ( -24.78791250444086458, 5.000000000000001776, -1.973611014893982940 ) ) ;
#7860 = CARTESIAN_POINT ( 'NONE',  ( 24.62111388750000174, 0.4562499990440845310, -10.19839929293505776 ) ) ;
#7861 = ORIENTED_EDGE ( 'NONE', *, *, #711, .T. ) ;
#7862 = CARTESIAN_POINT ( 'NONE',  ( -1.500000000000000444, 83.00000000000000000, -1.500000000000000222 ) ) ;
#7863 = PRESENTATION_STYLE_ASSIGNMENT (( #4378 ) ) ;
#7864 = CARTESIAN_POINT ( 'NONE',  ( 1.040834085586084257E-14, 88.00000000000001421, 0.000000000000000000 ) ) ;
#7865 = FACE_BOUND ( 'NONE', #582, .T. ) ;
#7866 = CARTESIAN_POINT ( 'NONE',  ( 17.67766952966368521, 1.487499998088169129, 17.67766952966369232 ) ) ;
#7867 = EDGE_LOOP ( 'NONE', ( #4805, #4653 ) ) ;
#7868 = ORIENTED_EDGE ( 'NONE', *, *, #2932, .T. ) ;
#7869 = CARTESIAN_POINT ( 'NONE',  ( -24.62111388750000174, 1.893749999044084475, -3.015216831376932151E-15 ) ) ;
#7870 = ORIENTED_EDGE ( 'NONE', *, *, #1732, .T. ) ;
#7871 = ADVANCED_FACE ( 'NONE', ( #5623 ), #592, .F. ) ;
#7872 = CARTESIAN_POINT ( 'NONE',  ( -2.999999999999999112, 25.00000000000000000, -19.75000000000000000 ) ) ;
#7873 = CARTESIAN_POINT ( 'NONE',  ( 17.40975659021752975, 1.343749999044084653, -17.40975659021752975 ) ) ;
#7874 = DIRECTION ( 'NONE',  ( 0.000000000000000000, -2.775557561562887961E-17, -1.000000000000000000 ) ) ;
#7875 = CARTESIAN_POINT ( 'NONE',  ( 17.67766952966368521, 2.487499998088169129, 17.67766952966369232 ) ) ;
#7876 = CARTESIAN_POINT ( 'NONE',  ( 1.530808498934191521E-15, 0.2500000000000000000, -25.00000000000000000 ) ) ;
#7877 = DIRECTION ( 'NONE',  ( -0.000000000000000000, 1.000000000000000000, 0.000000000000000000 ) ) ;
#7878 = DIRECTION ( 'NONE',  ( -1.000000000000000000, 0.000000000000000000, 0.000000000000000000 ) ) ;
#7879 = CARTESIAN_POINT ( 'NONE',  ( -5.276923788646491253, 28.00000000000000000, 15.13990010960497834 ) ) ;
#7880 = CARTESIAN_POINT ( 'NONE',  ( -10.35533905932739174, 4.687500000000000888, 24.99999999999999289 ) ) ;
#7881 = DIRECTION ( 'NONE',  ( -0.9819805060619644088, -0.000000000000000000, -0.1889822365046201491 ) ) ;
#7882 = ORIENTED_EDGE ( 'NONE', *, *, #8939, .F. ) ;
#7883 = ORIENTED_EDGE ( 'NONE', *, *, #4579, .F. ) ;
#7884 = ORIENTED_EDGE ( 'NONE', *, *, #9976, .T. ) ;
#7885 = EDGE_CURVE ( 'NONE', #7767, #1673, #1479, .T. ) ;
#7886 = DIRECTION ( 'NONE',  ( 0.000000000000000000, -2.775557561562888270E-17, -1.000000000000000000 ) ) ;
#7887 =( REPRESENTATION_RELATIONSHIP ('NONE','NONE', #1269, #5436 ) REPRESENTATION_RELATIONSHIP_WITH_TRANSFORMATION ( #10153 )SHAPE_REPRESENTATION_RELATIONSHIP( ) );
#7888 = DIRECTION ( 'NONE',  ( 0.000000000000000000, 0.000000000000000000, -1.000000000000000000 ) ) ;
#7889 = CARTESIAN_POINT ( 'NONE',  ( 0.000000000000000000, 85.00000000000000000, 0.000000000000000000 ) ) ;
#7890 = EDGE_CURVE ( 'NONE', #9231, #5941, #3788, .T. ) ;
#7891 = LINE ( 'NONE', #368, #64 ) ;
#7892 = DIRECTION ( 'NONE',  ( 0.000000000000000000, 1.000000000000000000, 0.000000000000000000 ) ) ;
#7893 = DIRECTION ( 'NONE',  ( 1.000000000000000000, 0.000000000000000000, 0.000000000000000000 ) ) ;
#7894 = DIRECTION ( 'NONE',  ( 0.000000000000000000, -2.775557561562887961E-17, -1.000000000000000000 ) ) ;
#7895 = CARTESIAN_POINT ( 'NONE',  ( 24.62111388749999463, 5.331249999044085364, 10.19839929293507730 ) ) ;
#7896 =( BOUNDED_CURVE ( )  B_SPLINE_CURVE ( 2, ( #630, #6343, #9029, #2186, #7363, #1463, #3153, #10638, #7168 ),
 .UNSPECIFIED., .F., .F. ) 
 B_SPLINE_CURVE_WITH_KNOTS ( ( 3, 2, 2, 2, 3 ),
 ( 0.6500000000000000222, 0.6750000000000000444, 0.6999999999999999556, 0.7249999999999999778, 0.7500000000000000000 ),
 .UNSPECIFIED. ) 
 CURVE ( )  GEOMETRIC_REPRESENTATION_ITEM ( )  RATIONAL_B_SPLINE_CURVE ( ( 1.000000000000000000, 0.9238795325112867385, 1.000000000000000000, 0.9238795325112867385, 1.000000000000000000, 0.9238795325112867385, 1.000000000000000000, 0.9238795325112867385, 1.000000000000000000 ) ) 
 REPRESENTATION_ITEM ( '' )  );
#7897 = VERTEX_POINT ( 'NONE', #3854 ) ;
#7898 = EDGE_CURVE ( 'NONE', #10325, #10901, #531, .T. ) ;
#7899 = VERTEX_POINT ( 'NONE', #9042 ) ;
#7900 = EDGE_CURVE ( 'NONE', #2289, #6733, #5355, .T. ) ;
#7901 = SURFACE_SIDE_STYLE ('',( #2846 ) ) ;
#7902 = CARTESIAN_POINT ( 'NONE',  ( 17.40975659021752620, 1.268749999044084475, 17.40975659021753330 ) ) ;
#7903 = DIRECTION ( 'NONE',  ( 0.000000000000000000, 0.000000000000000000, 1.000000000000000000 ) ) ;
#7904 = EDGE_CURVE ( 'NONE', #3864, #5936, #7653, .T. ) ;
#7905 = DIRECTION ( 'NONE',  ( -0.000000000000000000, -1.000000000000000000, -0.000000000000000000 ) ) ;
#7906 = CARTESIAN_POINT ( 'NONE',  ( 3.429011037612589276E-15, 85.00000000000000000, 28.00000000000000000 ) ) ;
#7907 = AXIS2_PLACEMENT_3D ( 'NONE', #7652, #1035, #6893 ) ;
#7908 = ORIENTED_EDGE ( 'NONE', *, *, #1213, .F. ) ;
#7909 = CARTESIAN_POINT ( 'NONE',  ( 2.999999999999999112, 25.00000000000000000, 19.75000000000000000 ) ) ;
#7910 = AXIS2_PLACEMENT_3D ( 'NONE', #10546, #7085, #4705 ) ;
#7911 = DIRECTION ( 'NONE',  ( 0.8660254037844450359, 0.000000000000000000, -0.4999999999999888978 ) ) ;
#7912 = LINE ( 'NONE', #2805, #5507 ) ;
#7913 = ORIENTED_EDGE ( 'NONE', *, *, #4702, .F. ) ;
#7914 = CARTESIAN_POINT ( 'NONE',  ( 0.000000000000000000, 10.00000000000000355, 0.000000000000000000 ) ) ;
#7915 = FACE_OUTER_BOUND ( 'NONE', #6485, .T. ) ;
#7916 = CARTESIAN_POINT ( 'NONE',  ( -17.40975659021753330, 4.843749999044083765, 17.40975659021752975 ) ) ;
#7917 = CARTESIAN_POINT ( 'NONE',  ( -4.592425496802574367E-15, 2.362499998088169129, 25.00000000000000000 ) ) ;
#7918 = ORIENTED_EDGE ( 'NONE', *, *, #3552, .F. ) ;
#7919 = VECTOR ( 'NONE', #3086, 1000.000000000000114 ) ;
#7920 = LINE ( 'NONE', #10513, #1758 ) ;
#7921 = CARTESIAN_POINT ( 'NONE',  ( 10.19839929293506486, 2.031249999044084653, 24.62111388749999819 ) ) ;
#7922 = CARTESIAN_POINT ( 'NONE',  ( -24.62111388750000174, 4.831249999044085364, -10.19839929293506131 ) ) ;
#7923 = CARTESIAN_POINT ( 'NONE',  ( 17.67766952966368521, 3.875000000000000000, 17.67766952966369232 ) ) ;
#7924 = DIRECTION ( 'NONE',  ( 0.000000000000000000, 0.000000000000000000, 1.000000000000000000 ) ) ;
#7925 = DIRECTION ( 'NONE',  ( -2.168404344971010347E-16, 0.000000000000000000, -1.000000000000000000 ) ) ;
#7926 = DIRECTION ( 'NONE',  ( 0.000000000000000000, -1.000000000000000000, 0.000000000000000000 ) ) ;
#7927 = CARTESIAN_POINT ( 'NONE',  ( -17.67766952966368876, 2.375000000000000000, -17.67766952966369232 ) ) ;
#7928 = CARTESIAN_POINT ( 'NONE',  ( -17.67766952966369232, 4.625000000000000000, 17.67766952966368876 ) ) ;
#7929 = CIRCLE ( 'NONE', #9510, 10.50000000000000000 ) ;
#7930 = ORIENTED_EDGE ( 'NONE', *, *, #5704, .F. ) ;
#7931 = DIRECTION ( 'NONE',  ( 0.000000000000000000, 0.000000000000000000, -1.000000000000000000 ) ) ;
#7932 = DIRECTION ( 'NONE',  ( -0.5000000000000073275, 0.000000000000000000, -0.8660254037844344888 ) ) ;
#7933 = CARTESIAN_POINT ( 'NONE',  ( 0.000000000000000000, 88.00000000000001421, 0.000000000000000000 ) ) ;
#7934 = CARTESIAN_POINT ( 'NONE',  ( -5.890223162633825282, 19.34316356887879707, -3.785909150703112402 ) ) ;
#7935 = EDGE_CURVE ( 'NONE', #1367, #8849, #2518, .T. ) ;
#7936 = CARTESIAN_POINT ( 'NONE',  ( 3.061616997868383043E-15, 5.000000000000000000, 25.00000000000000000 ) ) ;
#7937 = CARTESIAN_POINT ( 'NONE',  ( -25.00000000000001066, 1.562500000000000000, 10.35533905932737397 ) ) ;
#7938 = CARTESIAN_POINT ( 'NONE',  ( 24.62111388750000174, 4.393749999044084475, 0.000000000000000000 ) ) ;
#7939 = VERTEX_POINT ( 'NONE', #640 ) ;
#7940 = AXIS2_PLACEMENT_3D ( 'NONE', #7622, #1889, #3354 ) ;
#7941 = AXIS2_PLACEMENT_3D ( 'NONE', #3240, #9947, #5708 ) ;
#7942 = ADVANCED_FACE ( 'NONE', ( #2135 ), #4020, .T. ) ;
#7943 = ORIENTED_EDGE ( 'NONE', *, *, #5661, .F. ) ;
#7944 = PRODUCT_DEFINITION_SHAPE ( 'NONE', 'NONE',  #4432 ) ;
#7945 = CARTESIAN_POINT ( 'NONE',  ( 10.19839929293506486, 4.206249999044083587, 24.62111388749999819 ) ) ;
#7946 = CARTESIAN_POINT ( 'NONE',  ( 2.500000000000000444, -1.000000000000003109, -0.5773502691896260641 ) ) ;
#7947 = DIRECTION ( 'NONE',  ( 0.000000000000000000, 0.000000000000000000, -1.000000000000000000 ) ) ;
#7948 = CIRCLE ( 'NONE', #1071, 12.77350269189627063 ) ;
#7949 = VECTOR ( 'NONE', #10109, 1000.000000000000114 ) ;
#7950 = CYLINDRICAL_SURFACE ( 'NONE', #2168, 6.999999999999997335 ) ;
#7951 = ADVANCED_FACE ( 'NONE', ( #3160 ), #8983, .F. ) ;
#7952 = CYLINDRICAL_SURFACE ( 'NONE', #6563, 2.000000000000000000 ) ;
#7953 = EDGE_CURVE ( 'NONE', #2787, #8771, #2949, .T. ) ;
#7954 = ORIENTED_EDGE ( 'NONE', *, *, #6397, .F. ) ;
#7955 = EDGE_CURVE ( 'NONE', #9592, #5068, #1052, .T. ) ;
#7956 = VERTEX_POINT ( 'NONE', #5948 ) ;
#7957 = CIRCLE ( 'NONE', #9714, 5.100000000000006750 ) ;
#7958 = VECTOR ( 'NONE', #8209, 1000.000000000000000 ) ;
#7959 = CARTESIAN_POINT ( 'NONE',  ( -24.62111388750000174, 4.831249999044084475, -10.19839929293506131 ) ) ;
#7960 = DIRECTION ( 'NONE',  ( 1.000000000000000000, 0.000000000000000000, -0.000000000000000000 ) ) ;
#7961 = CARTESIAN_POINT ( 'NONE',  ( -24.64992079640905587, 4.999999999999998224, -3.388298626009401460 ) ) ;
#7962 = CARTESIAN_POINT ( 'NONE',  ( -1.500000000000001332, 5.750000000000006217, -2.168404344971008868E-16 ) ) ;
#7963 = VERTEX_POINT ( 'NONE', #5024 ) ;
#7964 = LINE ( 'NONE', #341, #6550 ) ;
#7965 = DIRECTION ( 'NONE',  ( 0.000000000000000000, 0.000000000000000000, -1.000000000000000000 ) ) ;
#7966 = ORIENTED_EDGE ( 'NONE', *, *, #7258, .F. ) ;
#7967 = CARTESIAN_POINT ( 'NONE',  ( 24.62111388750000174, 2.281249999044085541, -10.19839929293505776 ) ) ;
#7968 = CARTESIAN_POINT ( 'NONE',  ( 24.99999999999999289, 2.549999998088169129, 10.35533905932739529 ) ) ;
#7969 = VECTOR ( 'NONE', #6363, 1000.000000000000000 ) ;
#7970 = VERTEX_POINT ( 'NONE', #3446 ) ;
#7971 = EDGE_CURVE ( 'NONE', #2327, #7970, #7597, .T. ) ;
#7972 = CARTESIAN_POINT ( 'NONE',  ( -20.63749999999999929, 8.299669118052633340E-16, 5.525000000000006573 ) ) ;
#7973 = CARTESIAN_POINT ( 'NONE',  ( 24.62111388750000174, 4.218749999044084653, 0.000000000000000000 ) ) ;
#7974 = CARTESIAN_POINT ( 'NONE',  ( 10.19839929293506486, 2.206249999044084920, 24.62111388749999819 ) ) ;
#7975 = CARTESIAN_POINT ( 'NONE',  ( -17.67766952966368876, 4.375000000000000000, -17.67766952966369232 ) ) ;
#7976 = CARTESIAN_POINT ( 'NONE',  ( 6.296693311223896750, 10.00000000000000355, 3.058047309050043960 ) ) ;
#7977 = LINE ( 'NONE', #6277, #364 ) ;
#7978 = CARTESIAN_POINT ( 'NONE',  ( 24.81055694375000087, 5.503124998566127246, 0.000000000000000000 ) ) ;
#7979 = CARTESIAN_POINT ( 'NONE',  ( 67.07963283087528339, 92.45240317130979690, -5.000000000000000000 ) ) ;
#7980 = CARTESIAN_POINT ( 'NONE',  ( 25.00000000000000000, 2.062500000000000000, -10.35533905932737753 ) ) ;
#7981 = AXIS2_PLACEMENT_3D ( 'NONE', #6296, #10647, #3852 ) ;
#7982 = ORIENTED_EDGE ( 'NONE', *, *, #4771, .T. ) ;
#7983 = ORIENTED_EDGE ( 'NONE', *, *, #2523, .F. ) ;
#7984 = VECTOR ( 'NONE', #5709, 1000.000000000000114 ) ;
#7985 = DIRECTION ( 'NONE',  ( 1.000000000000000000, 0.000000000000000000, -1.224646799147353207E-16 ) ) ;
#7986 = FACE_OUTER_BOUND ( 'NONE', #8560, .T. ) ;
#7987 = DIRECTION ( 'NONE',  ( -1.000000000000000000, -0.000000000000000000, -0.000000000000000000 ) ) ;
#7988 = AXIS2_PLACEMENT_3D ( 'NONE', #1204, #3682, #264 ) ;
#7989 = CARTESIAN_POINT ( 'NONE',  ( 5.437177826491049082, 19.75000000000000355, 3.716506350946132020 ) ) ;
#7990 = VECTOR ( 'NONE', #817, 1000.000000000000114 ) ;
#7991 = DIRECTION ( 'NONE',  ( 0.000000000000000000, 0.000000000000000000, 1.000000000000000000 ) ) ;
#7992 = CARTESIAN_POINT ( 'NONE',  ( 2.999999999999999112, 28.00000000000000000, 19.75000000000000000 ) ) ;
#7993 = EDGE_LOOP ( 'NONE', ( #5658, #7334, #6717, #562 ) ) ;
#7994 = AXIS2_PLACEMENT_3D ( 'NONE', #2476, #5865, #7143 ) ;
#7995 = ORIENTED_EDGE ( 'NONE', *, *, #2321, .T. ) ;
#7996 = AXIS2_PLACEMENT_3D ( 'NONE', #8997, #7505, #10666 ) ;
#7997 = EDGE_LOOP ( 'NONE', ( #1655, #8886, #1469, #1007 ) ) ;
#7998 = CIRCLE ( 'NONE', #4291, 2.000000000000004441 ) ;
#7999 = CYLINDRICAL_SURFACE ( 'NONE', #2495, 25.00000000000000000 ) ;
#8000 = CIRCLE ( 'NONE', #3208, 25.00000000000000000 ) ;
#8001 = CYLINDRICAL_SURFACE ( 'NONE', #10648, 25.00000000000000000 ) ;
#8002 = AXIS2_PLACEMENT_3D ( 'NONE', #7598, #2555, #25 ) ;
#8003 = DIRECTION ( 'NONE',  ( 0.6123724356957986892, -0.3535533905932728427, -0.7071067811865445751 ) ) ;
#8004 = CARTESIAN_POINT ( 'NONE',  ( 9.875000000000023093, -0.001000000000001000089, 20.10400172474264835 ) ) ;
#8005 = CARTESIAN_POINT ( 'NONE',  ( -5.000000000000000000, 93.00000000000001421, 0.000000000000000000 ) ) ;
#8006 = AXIS2_PLACEMENT_3D ( 'NONE', #472, #6490, #8972 ) ;
#8007 = ORIENTED_EDGE ( 'NONE', *, *, #1960, .T. ) ;
#8008 = ADVANCED_FACE ( 'NONE', ( #8422 ), #10307, .T. ) ;
#8009 = EDGE_CURVE ( 'NONE', #3376, #5115, #1822, .T. ) ;
#8010 = CARTESIAN_POINT ( 'NONE',  ( 0.000000000000000000, 0.000000000000000000, 0.000000000000000000 ) ) ;
#8011 = FACE_OUTER_BOUND ( 'NONE', #4695, .T. ) ;
#8012 = DIRECTION ( 'NONE',  ( -0.7071067811865470176, 0.3535533905932748411, 0.6123724356957946924 ) ) ;
#8013 = CARTESIAN_POINT ( 'NONE',  ( 10.19839929293505953, 2.581249999044084920, -24.62111388750000174 ) ) ;
#8014 = VERTEX_POINT ( 'NONE', #6786 ) ;
#8015 = CARTESIAN_POINT ( 'NONE',  ( -5.937177826491102373, 19.75000000000001066, 2.850480947161618595 ) ) ;
#8016 = CARTESIAN_POINT ( 'NONE',  ( -4.592425496802574367E-15, 2.750000000000000000, 25.00000000000000000 ) ) ;
#8017 = CARTESIAN_POINT ( 'NONE',  ( 2.472467130856905282, 4.983902298070619352, 24.62111388750000174 ) ) ;
#8018 = DIRECTION ( 'NONE',  ( -0.3273268353539878217, 0.000000000000000000, 0.9449111825230682715 ) ) ;
#8019 = ADVANCED_FACE ( 'NONE', ( #23 ), #10027, .T. ) ;
#8020 = ORIENTED_EDGE ( 'NONE', *, *, #7395, .T. ) ;
#8021 = ORIENTED_EDGE ( 'NONE', *, *, #1676, .F. ) ;
#8022 = EDGE_CURVE ( 'NONE', #3515, #1394, #1998, .T. ) ;
#8023 = CARTESIAN_POINT ( 'NONE',  ( -0.1668442477450440553, 19.66631150450991328, -6.999999999999995559 ) ) ;
#8024 = CARTESIAN_POINT ( 'NONE',  ( 24.62111388750000174, 3.281249999044085097, -10.19839929293505776 ) ) ;
#8025 = CARTESIAN_POINT ( 'NONE',  ( -24.62111388750000884, 4.956249999044084475, 10.19839929293505421 ) ) ;
#8026 = VERTEX_POINT ( 'NONE', #2554 ) ;
#8027 = CARTESIAN_POINT ( 'NONE',  ( -10.35533905932737575, 2.312500000000000888, -25.00000000000000000 ) ) ;
#8028 = CYLINDRICAL_SURFACE ( 'NONE', #9130, 5.000000000000005329 ) ;
#8029 = CARTESIAN_POINT ( 'NONE',  ( 17.67766952966369232, 1.737499998088169351, -17.67766952966369232 ) ) ;
#8030 = PRODUCT_DEFINITION_CONTEXT ( 'detailed design', #673, 'design' ) ;
#8031 = CARTESIAN_POINT ( 'NONE',  ( -6.305607966083712768, 7.781088913245557848, -11.92163336986838473 ) ) ;
#8032 = CARTESIAN_POINT ( 'NONE',  ( 10.35533905932739174, 0.8125000000000001110, 24.99999999999998934 ) ) ;
#8033 = ADVANCED_FACE ( 'NONE', ( #755 ), #3387, .F. ) ;
#8034 = ORIENTED_EDGE ( 'NONE', *, *, #3331, .F. ) ;
#8035 = ORIENTED_EDGE ( 'NONE', *, *, #9372, .T. ) ;
#8036 = ORIENTED_EDGE ( 'NONE', *, *, #9560, .T. ) ;
#8037 = ORIENTED_EDGE ( 'NONE', *, *, #7355, .T. ) ;
#8038 = UNCERTAINTY_MEASURE_WITH_UNIT (LENGTH_MEASURE( 1.000000000000000082E-05 ), #3651, 'distance_accuracy_value', 'NONE');
#8039 = LINE ( 'NONE', #468, #9002 ) ;
#8040 = CARTESIAN_POINT ( 'NONE',  ( -15.75000000000000000, -0.001000000000001000089, 1.681956355172181189E-13 ) ) ;
#8041 = CARTESIAN_POINT ( 'NONE',  ( 5.978755702618532730, 19.66631150450991328, 3.644491357022537237 ) ) ;
#8042 =( BOUNDED_CURVE ( )  B_SPLINE_CURVE ( 2, ( #3398, #993, #4359, #6912, #3517, #3336, #5029, #216, #6972 ),
 .UNSPECIFIED., .F., .F. ) 
 B_SPLINE_CURVE_WITH_KNOTS ( ( 3, 2, 2, 2, 3 ),
 ( 0.6500000000000000222, 0.6750000000000000444, 0.6999999999999999556, 0.7249999999999999778, 0.7500000000000000000 ),
 .UNSPECIFIED. ) 
 CURVE ( )  GEOMETRIC_REPRESENTATION_ITEM ( )  RATIONAL_B_SPLINE_CURVE ( ( 1.000000000000000000, 0.9238795325112867385, 1.000000000000000000, 0.9238795325112867385, 1.000000000000000000, 0.9238795325112867385, 1.000000000000000000, 0.9238795325112867385, 1.000000000000000000 ) ) 
 REPRESENTATION_ITEM ( '' )  );
#8043 = CARTESIAN_POINT ( 'NONE',  ( 3.223142256880076948E-15, -0.001000000000001000089, 15.75000000000000000 ) ) ;
#8044 = ORIENTED_EDGE ( 'NONE', *, *, #1331, .F. ) ;
#8045 = ORIENTED_EDGE ( 'NONE', *, *, #1203, .T. ) ;
#8046 = CARTESIAN_POINT ( 'NONE',  ( -1.500000000000001776, -1.415534356397074737E-16, -5.100000000000006750 ) ) ;
#8047 = DIRECTION ( 'NONE',  ( 0.000000000000000000, -1.000000000000000000, 0.000000000000000000 ) ) ;
#8048 = CARTESIAN_POINT ( 'NONE',  ( 6.982120021884469452, 10.00000000000000355, -0.4999999999999756306 ) ) ;
#8049 = CARTESIAN_POINT ( 'NONE',  ( -10.00000000000000000, 90.00000000000001421, -5.000000000000000000 ) ) ;
#8050 = FACE_OUTER_BOUND ( 'NONE', #6953, .T. ) ;
#8051 = ORIENTED_EDGE ( 'NONE', *, *, #9514, .F. ) ;
#8052 = DIRECTION ( 'NONE',  ( -1.000000000000000000, 0.000000000000000000, 2.168404344971010347E-16 ) ) ;
#8053 = CARTESIAN_POINT ( 'NONE',  ( -22.18568234790235039, 4.999999999999997335, -11.47449125965302841 ) ) ;
#8054 = CARTESIAN_POINT ( 'NONE',  ( 24.62111388750000174, 5.393749999044085364, 0.000000000000000000 ) ) ;
#8055 = EDGE_LOOP ( 'NONE', ( #2205, #259, #242, #3440 ) ) ;
#8056 = LINE ( 'NONE', #9770, #3714 ) ;
#8057 = CYLINDRICAL_SURFACE ( 'NONE', #2507, 2.000000000000004441 ) ;
#8058 = ORIENTED_EDGE ( 'NONE', *, *, #4211, .T. ) ;
#8059 =( GEOMETRIC_REPRESENTATION_CONTEXT ( 3 ) GLOBAL_UNCERTAINTY_ASSIGNED_CONTEXT ( ( #8356 ) ) GLOBAL_UNIT_ASSIGNED_CONTEXT ( ( #6637, #9995, #6586 ) ) REPRESENTATION_CONTEXT ( 'NONE', 'WORKASPACE' ) );
#8060 = CARTESIAN_POINT ( 'NONE',  ( 24.62111388750000174, 2.218749999044084653, 0.000000000000000000 ) ) ;
#8061 = CARTESIAN_POINT ( 'NONE',  ( 1.530808498934191521E-15, 0.2500000000000000000, -25.00000000000000000 ) ) ;
#8062 = EDGE_CURVE ( 'NONE', #8354, #7707, #1447, .T. ) ;
#8063 = VERTEX_POINT ( 'NONE', #5125 ) ;
#8064 = EDGE_CURVE ( 'NONE', #9935, #6450, #4794, .T. ) ;
#8065 = EDGE_LOOP ( 'NONE', ( #1956, #2256, #7748, #8084, #4173, #9969 ) ) ;
#8066 = AXIS2_PLACEMENT_3D ( 'NONE', #5525, #8012, #6416 ) ;
#8067 = EDGE_CURVE ( 'NONE', #3676, #6596, #5541, .T. ) ;
#8068 = DIRECTION ( 'NONE',  ( -0.3273268353539845466, -0.000000000000000000, -0.9449111825230696038 ) ) ;
#8069 = CARTESIAN_POINT ( 'NONE',  ( -24.62111388750000174, 4.656249999044085541, -10.19839929293506131 ) ) ;
#8070 = AXIS2_PLACEMENT_3D ( 'NONE', #8475, #6833, #6003 ) ;
#8071 = CARTESIAN_POINT ( 'NONE',  ( -17.40975659021752975, 3.768749999044084475, -17.40975659021752975 ) ) ;
#8072 = ORIENTED_EDGE ( 'NONE', *, *, #9720, .F. ) ;
#8073 = CARTESIAN_POINT ( 'NONE',  ( 25.00000000000000000, 4.000000000000000000, 0.000000000000000000 ) ) ;
#8074 =( NAMED_UNIT ( * ) PLANE_ANGLE_UNIT ( ) SI_UNIT ( $, .RADIAN. ) );
#8075 = CARTESIAN_POINT ( 'NONE',  ( 82.32050807568876394, 92.28203230275514102, 0.000000000000000000 ) ) ;
#8076 = DIRECTION ( 'NONE',  ( -0.4330127018922172999, -0.8660254037844380415, -0.2500000000000055511 ) ) ;
#8077 = DIRECTION ( 'NONE',  ( 0.000000000000000000, 1.000000000000000000, 0.000000000000000000 ) ) ;
#8078 = CARTESIAN_POINT ( 'NONE',  ( 24.99999999999999289, 3.549999998088169573, 10.35533905932739529 ) ) ;
#8079 = STYLED_ITEM ( 'NONE', ( #2922 ), #9554 ) ;
#8080 = EDGE_CURVE ( 'NONE', #1429, #10131, #7491, .T. ) ;
#8081 = ORIENTED_EDGE ( 'NONE', *, *, #845, .T. ) ;
#8082 = EDGE_LOOP ( 'NONE', ( #4172, #6807, #6311, #9030 ) ) ;
#8083 = ORIENTED_EDGE ( 'NONE', *, *, #1166, .F. ) ;
#8084 = ORIENTED_EDGE ( 'NONE', *, *, #585, .T. ) ;
#8085 = ADVANCED_FACE ( 'NONE', ( #4179 ), #6008, .F. ) ;
#8086 = LINE ( 'NONE', #1930, #2302 ) ;
#8087 = DIRECTION ( 'NONE',  ( 0.000000000000000000, 0.000000000000000000, -1.000000000000000000 ) ) ;
#8088 = DIRECTION ( 'NONE',  ( 0.000000000000000000, -1.000000000000000000, 0.000000000000000000 ) ) ;
#8089 = DIRECTION ( 'NONE',  ( 0.000000000000000000, 0.000000000000000000, 1.000000000000000000 ) ) ;
#8090 = CARTESIAN_POINT ( 'NONE',  ( 1.040834085586084257E-14, 90.00000000000001421, -4.999999999999987566 ) ) ;
#8091 = DIRECTION ( 'NONE',  ( 0.000000000000000000, 1.000000000000000000, 0.000000000000000000 ) ) ;
#8092 = CARTESIAN_POINT ( 'NONE',  ( 3.061616997868383043E-15, 85.00000000000000000, 25.00000000000000000 ) ) ;
#8093 = ORIENTED_EDGE ( 'NONE', *, *, #3787, .F. ) ;
#8094 = EDGE_CURVE ( 'NONE', #8246, #4894, #4902, .T. ) ;
#8095 = ORIENTED_EDGE ( 'NONE', *, *, #7670, .F. ) ;
#8096 =( GEOMETRIC_REPRESENTATION_CONTEXT ( 3 ) GLOBAL_UNCERTAINTY_ASSIGNED_CONTEXT ( ( #8236 ) ) GLOBAL_UNIT_ASSIGNED_CONTEXT ( ( #769, #6513, #8994 ) ) REPRESENTATION_CONTEXT ( 'NONE', 'WORKASPACE' ) );
#8097 = DIRECTION ( 'NONE',  ( 0.000000000000000000, -2.775557561562887961E-17, -1.000000000000000000 ) ) ;
#8098 = DIRECTION ( 'NONE',  ( -0.000000000000000000, 1.000000000000000000, -0.000000000000000000 ) ) ;
#8099 = CARTESIAN_POINT ( 'NONE',  ( 0.000000000000000000, 0.000000000000000000, 0.000000000000000000 ) ) ;
#8100 = PLANE ( 'NONE',  #4301 ) ;
#8101 = DIRECTION ( 'NONE',  ( -0.000000000000000000, -1.000000000000000000, -0.000000000000000000 ) ) ;
#8102 = AXIS2_PLACEMENT_3D ( 'NONE', #7555, #7439, #10826 ) ;
#8103 = VERTEX_POINT ( 'NONE', #5779 ) ;
#8104 = VERTEX_POINT ( 'NONE', #10925 ) ;
#8105 = AXIS2_PLACEMENT_3D ( 'NONE', #6623, #1372, #653 ) ;
#8106 = CARTESIAN_POINT ( 'NONE',  ( -4.592425496802574367E-15, 4.750000000000000000, 25.00000000000000000 ) ) ;
#8107 = CARTESIAN_POINT ( 'NONE',  ( -3.924072712834378862, 10.00000000000000355, -5.796693311223959810 ) ) ;
#8108 = VECTOR ( 'NONE', #7418, 1000.000000000000000 ) ;
#8109 = CARTESIAN_POINT ( 'NONE',  ( 24.62111388750000174, 2.393749999044084475, 0.000000000000000000 ) ) ;
#8110 = ORIENTED_EDGE ( 'NONE', *, *, #3823, .T. ) ;
#8111 = DIRECTION ( 'NONE',  ( -0.000000000000000000, -1.000000000000000000, -0.000000000000000000 ) ) ;
#8112 = SURFACE_STYLE_USAGE ( .BOTH. , #6364 ) ;
#8113 = DIRECTION ( 'NONE',  ( 7.228014483236695816E-17, 0.000000000000000000, -1.000000000000000000 ) ) ;
#8114 = ORIENTED_EDGE ( 'NONE', *, *, #4903, .F. ) ;
#8115 = CARTESIAN_POINT ( 'NONE',  ( -17.40975659021752975, 3.593749999044084653, -17.40975659021752975 ) ) ;
#8116 = CARTESIAN_POINT ( 'NONE',  ( 25.00000000000000000, 4.062500000000000000, -10.35533905932737753 ) ) ;
#8117 = VECTOR ( 'NONE', #928, 1000.000000000000000 ) ;
#8118 = VERTEX_POINT ( 'NONE', #6725 ) ;
#8119 = CIRCLE ( 'NONE', #10060, 24.91176187412963117 ) ;
#8120 = ORIENTED_EDGE ( 'NONE', *, *, #10324, .T. ) ;
#8121 = CARTESIAN_POINT ( 'NONE',  ( 24.99999999999999289, 4.549999998088169129, 10.35533905932739529 ) ) ;
#8122 = CARTESIAN_POINT ( 'NONE',  ( 0.1920286436967143240, 5.812771276357657970E-16, -5.525000000000000355 ) ) ;
#8123 = CARTESIAN_POINT ( 'NONE',  ( -24.62111388750000174, 2.831249999044084475, -10.19839929293506131 ) ) ;
#8124 = PRODUCT_DEFINITION ( 'UNKNOWN', '', #4418, #9123 ) ;
#8125 = EDGE_CURVE ( 'NONE', #8014, #10892, #3591, .T. ) ;
#8126 = CARTESIAN_POINT ( 'NONE',  ( 17.67766952966368521, 1.875000000000000000, 17.67766952966369232 ) ) ;
#8127 = AXIS2_PLACEMENT_3D ( 'NONE', #4401, #4575, #1193 ) ;
#8128 = VECTOR ( 'NONE', #4865, 1000.000000000000000 ) ;
#8129 = CYLINDRICAL_SURFACE ( 'NONE', #2946, 28.00000000000000000 ) ;
#8130 = DIRECTION ( 'NONE',  ( 0.3061862178479012875, -0.3535533905932726761, 0.8838834764831834390 ) ) ;
#8131 = DIRECTION ( 'NONE',  ( 0.3061862178479106134, 0.3535533905932737864, -0.8838834764831797752 ) ) ;
#8132 = CARTESIAN_POINT ( 'NONE',  ( 17.67766952966368521, 0.8750000000000000000, 17.67766952966369232 ) ) ;
#8133 = EDGE_CURVE ( 'NONE', #4397, #8924, #5019, .T. ) ;
#8134 = ORIENTED_EDGE ( 'NONE', *, *, #6722, .T. ) ;
#8135 = ORIENTED_EDGE ( 'NONE', *, *, #6063, .T. ) ;
#8136 = EDGE_LOOP ( 'NONE', ( #10493, #6988, #10509, #5053 ) ) ;
#8137 = EDGE_LOOP ( 'NONE', ( #9423, #2016, #6989, #5818 ) ) ;
#8138 = UNCERTAINTY_MEASURE_WITH_UNIT (LENGTH_MEASURE( 1.000000000000000082E-05 ), #2638, 'distance_accuracy_value', 'NONE');
#8139 = AXIS2_PLACEMENT_3D ( 'NONE', #3097, #6445, #9798 ) ;
#8140 = ADVANCED_FACE ( 'NONE', ( #2781 ), #2671, .T. ) ;
#8141 = EDGE_CURVE ( 'NONE', #620, #7707, #5247, .T. ) ;
#8142 = DIRECTION ( 'NONE',  ( 1.000000000000000000, 0.000000000000000000, 0.000000000000000000 ) ) ;
#8143 = EDGE_CURVE ( 'NONE', #10668, #4321, #7891, .T. ) ;
#8144 = DIRECTION ( 'NONE',  ( 0.000000000000000000, 0.000000000000000000, -1.000000000000000000 ) ) ;
#8145 = CARTESIAN_POINT ( 'NONE',  ( 0.000000000000000000, 25.00000000000000355, -2.000000000000000000 ) ) ;
#8146 = LINE ( 'NONE', #6341, #10078 ) ;
#8147 = CARTESIAN_POINT ( 'NONE',  ( 0.000000000000000000, -1.026060429977008193, 0.000000000000000000 ) ) ;
#8148 = LINE ( 'NONE', #9082, #6938 ) ;
#8149 = EDGE_CURVE ( 'NONE', #10544, #620, #10459, .T. ) ;
#8150 = CIRCLE ( 'NONE', #9907, 12.77350269189627063 ) ;
#8151 = AXIS2_PLACEMENT_3D ( 'NONE', #766, #1582, #7435 ) ;
#8152 = ORIENTED_EDGE ( 'NONE', *, *, #256, .T. ) ;
#8153 = EDGE_CURVE ( 'NONE', #4266, #6402, #4650, .T. ) ;
#8154 = AXIS2_PLACEMENT_3D ( 'NONE', #3268, #4961, #6669 ) ;
#8155 = AXIS2_PLACEMENT_3D ( 'NONE', #4749, #5734, #7272 ) ;
#8156 = CARTESIAN_POINT ( 'NONE',  ( 1.530808498934191521E-15, 1.250000000000000000, -25.00000000000000000 ) ) ;
#8157 = DIRECTION ( 'NONE',  ( 0.000000000000000000, -0.8660254037844380415, 0.5000000000000009992 ) ) ;
#8158 = DIRECTION ( 'NONE',  ( 0.000000000000000000, 1.000000000000000000, 0.000000000000000000 ) ) ;
#8159 = CARTESIAN_POINT ( 'NONE',  ( 17.67766952966369232, 0.1249999999999999722, -17.67766952966369232 ) ) ;
#8160 = DIRECTION ( 'NONE',  ( -0.000000000000000000, 1.000000000000000000, -0.000000000000000000 ) ) ;
#8161 = CIRCLE ( 'NONE', #10628, 2.999999999999998668 ) ;
#8162 = ADVANCED_FACE ( 'NONE', ( #10366 ), #1981, .F. ) ;
#8163 = CIRCLE ( 'NONE', #947, 6.999999999999997335 ) ;
#8164 = ORIENTED_EDGE ( 'NONE', *, *, #6287, .T. ) ;
#8165 =( BOUNDED_CURVE ( )  B_SPLINE_CURVE ( 3, ( #1853, #301, #1026, #10407 ),
 .UNSPECIFIED., .F., .F. ) 
 B_SPLINE_CURVE_WITH_KNOTS ( ( 4, 4 ),
 ( 2.284520705739659263, 2.356010155625180680 ),
 .UNSPECIFIED. ) 
 CURVE ( )  GEOMETRIC_REPRESENTATION_ITEM ( )  RATIONAL_B_SPLINE_CURVE ( ( 1.000000000000000000, 0.9995741502243209453, 0.9995741502243209453, 1.000000000000000000 ) ) 
 REPRESENTATION_ITEM ( '' )  );
#8166 = AXIS2_PLACEMENT_3D ( 'NONE', #7025, #7855, #4550 ) ;
#8167 = FILL_AREA_STYLE ('',( #541 ) ) ;
#8168 = DIRECTION ( 'NONE',  ( 0.000000000000000000, -1.000000000000000000, 0.000000000000000000 ) ) ;
#8169 = CARTESIAN_POINT ( 'NONE',  ( -17.40975659021752975, 3.768749999044084475, -17.40975659021752975 ) ) ;
#8170 = ORIENTED_EDGE ( 'NONE', *, *, #7314, .T. ) ;
#8171 = CARTESIAN_POINT ( 'NONE',  ( 0.000000000000000000, 10.00000000000000355, 0.000000000000000000 ) ) ;
#8172 = APPLICATION_PROTOCOL_DEFINITION ( 'draft international standard', 'automotive_design', 1998, #330 ) ;
#8173 = DIRECTION ( 'NONE',  ( 0.000000000000000000, 0.000000000000000000, -1.000000000000000000 ) ) ;
#8174 = VECTOR ( 'NONE', #7230, 1000.000000000000000 ) ;
#8175 = CARTESIAN_POINT ( 'NONE',  ( -10.35533905932737575, 1.312500000000000222, -25.00000000000000000 ) ) ;
#8176 = AXIS2_PLACEMENT_3D ( 'NONE', #10649, #3058, #590 ) ;
#8177 = ORIENTED_EDGE ( 'NONE', *, *, #66, .T. ) ;
#8178 = EDGE_LOOP ( 'NONE', ( #10151, #3674, #2736, #5043 ) ) ;
#8179 = AXIS2_PLACEMENT_3D ( 'NONE', #2043, #2850, #1217 ) ;
#8180 = CARTESIAN_POINT ( 'NONE',  ( -17.67766952966369232, 3.237499998088169573, 17.67766952966368876 ) ) ;
#8181 = PLANE ( 'NONE',  #4239 ) ;
#8182 = CARTESIAN_POINT ( 'NONE',  ( 24.62111388749999463, 2.156249999044085097, 10.19839929293507730 ) ) ;
#8183 = ORIENTED_EDGE ( 'NONE', *, *, #10512, .T. ) ;
#8184 = CARTESIAN_POINT ( 'NONE',  ( -25.00000000000000000, 2.049999998088169129, -10.35533905932738108 ) ) ;
#8185 = FACE_OUTER_BOUND ( 'NONE', #9993, .T. ) ;
#8186 = DIRECTION ( 'NONE',  ( 0.000000000000000000, -1.000000000000000000, 0.000000000000000000 ) ) ;
#8187 = DIRECTION ( 'NONE',  ( 0.4330127018922191318, -0.8660254037844380415, 0.2500000000000024980 ) ) ;
#8188 = ORIENTED_EDGE ( 'NONE', *, *, #446, .T. ) ;
#8189 = VERTEX_POINT ( 'NONE', #983 ) ;
#8190 = ORIENTED_EDGE ( 'NONE', *, *, #6268, .F. ) ;
#8191 = CARTESIAN_POINT ( 'NONE',  ( 1.507608415688466075E-15, 1.468749999044084431, -24.62111388750000174 ) ) ;
#8192 = FACE_OUTER_BOUND ( 'NONE', #10914, .T. ) ;
#8193 = ORIENTED_EDGE ( 'NONE', *, *, #7336, .T. ) ;
#8194 = DIRECTION ( 'NONE',  ( -0.000000000000000000, -1.000000000000000000, -0.000000000000000000 ) ) ;
#8195 = FACE_OUTER_BOUND ( 'NONE', #2189, .T. ) ;
#8196 = CARTESIAN_POINT ( 'NONE',  ( -17.40975659021752975, 1.593749999044084431, -17.40975659021752975 ) ) ;
#8197 = DIRECTION ( 'NONE',  ( 0.000000000000000000, -1.000000000000000000, 0.000000000000000000 ) ) ;
#8198 = EDGE_CURVE ( 'NONE', #6576, #122, #1815, .T. ) ;
#8199 = ORIENTED_EDGE ( 'NONE', *, *, #10120, .F. ) ;
#8200 = EDGE_CURVE ( 'NONE', #7140, #6576, #933, .T. ) ;
#8201 = CARTESIAN_POINT ( 'NONE',  ( -13.63990010960498367, 25.00000000000000000, -7.874999999999870326 ) ) ;
#8202 = CYLINDRICAL_SURFACE ( 'NONE', #8176, 5.000000000000004441 ) ;
#8203 = DIRECTION ( 'NONE',  ( 0.000000000000000000, 0.000000000000000000, -1.000000000000000000 ) ) ;
#8204 = DIRECTION ( 'NONE',  ( -0.000000000000000000, 1.000000000000000000, -0.000000000000000000 ) ) ;
#8205 = ADVANCED_FACE ( 'NONE', ( #1920 ), #9543, .F. ) ;
#8206 = ORIENTED_EDGE ( 'NONE', *, *, #7846, .T. ) ;
#8207 = ORIENTED_EDGE ( 'NONE', *, *, #8407, .F. ) ;
#8208 = ADVANCED_FACE ( 'NONE', ( #2837 ), #10481, .T. ) ;
#8209 = DIRECTION ( 'NONE',  ( 0.000000000000000000, 1.000000000000000000, -0.000000000000000000 ) ) ;
#8210 = CARTESIAN_POINT ( 'NONE',  ( 17.40975659021752620, 3.268749999044084475, 17.40975659021753330 ) ) ;
#8211 = ORIENTED_EDGE ( 'NONE', *, *, #8685, .F. ) ;
#8212 = DIRECTION ( 'NONE',  ( 0.8660254037844361541, 0.000000000000000000, -0.5000000000000042188 ) ) ;
#8213 = PRODUCT_CONTEXT ( 'NONE', #9136, 'mechanical' ) ;
#8214 = CARTESIAN_POINT ( 'NONE',  ( 0.000000000000000000, 5.000000000000000000, 0.000000000000000000 ) ) ;
#8215 = EDGE_LOOP ( 'NONE', ( #6626, #4910, #2801, #9120, #6388, #496 ) ) ;
#8216 = DIRECTION ( 'NONE',  ( 1.000000000000000000, 0.000000000000000000, 0.000000000000000000 ) ) ;
#8217 = CARTESIAN_POINT ( 'NONE',  ( 10.19839929293505953, 1.406249999044084209, -24.62111388750000174 ) ) ;
#8218 = ORIENTED_EDGE ( 'NONE', *, *, #4721, .F. ) ;
#8219 = VERTEX_POINT ( 'NONE', #6124 ) ;
#8220 =( BOUNDED_SURFACE ( )  B_SPLINE_SURFACE ( 1, 2, ( 
 ( #3465, #5969, #6856, #886, #4316, #164, #2631, #4255, #4370, #7735, #10335, #51, #3410, #10160, #10277, #2695, #950, #6028, #9388, #6091, #8614, #1059, #7796, #228, #7869, #293, #3658, #6156, #9522, #10868, #8457, #904, #7576, #4390, #2761, #2646, #6046, #9405, #7752, #5167, #9468, #2594, #3544, #10176, #9341, #6992, #1727, #1846, #1786, #5932, #245, #4454, #5103, #6107, #5988, #6819, #1021, #1900, #4271, #5229, #5281, #8516, #8572, #184, #4213, #6937, #7636, #969, #10297, #8629, #2539, #2711, #4333, #7696, #1078, #125, #7812, #3604, #9282, #10348, #6160 ),
 ( #9525, #3486, #5058, #8402, #844, #7, #3367, #6767, #10127, #6876, #10234, #72, #3427, #5391, #3825, #4566, #2970, #3721, #7873, #6376, #8691, #9682, #9730, #6316, #10514, #1138, #5334, #6218, #349, #7921, #10402, #3778, #1961, #7099, #2820, #10461, #503, #8747, #404, #2876, #4717, #2057, #9630, #7192, #5543, #3874, #1291, #6273, #5433, #8024, #4517, #8796, #10560, #4674, #2919, #7150, #296, #2105, #1235, #2159, #4618, #3661, #7044, #5483, #7973, #1186, #9578, #6430, #455, #8903, #1338, #8069, #8847, #7242, #2019, #10613, #3029, #9108, #3182, #8276, #1495 ) ),
 .UNSPECIFIED., .F., .F., .F. ) 
 B_SPLINE_SURFACE_WITH_KNOTS ( ( 2, 2 ),
 ( 3, 2, 2, 2, 2, 2, 2, 2, 2, 2, 2, 2, 2, 2, 2, 2, 2, 2, 2, 2, 2, 2, 2, 2, 2, 2, 2, 2, 2, 2, 2, 2, 2, 2, 2, 2, 2, 2, 2, 2, 3 ),
 ( 0.000000000000000000, 1.000000000000000000 ),
 ( 0.000000000000000000, 0.02500000000000000139, 0.05000000000000000278, 0.07499999999999999722, 0.1000000000000000056, 0.1250000000000000000, 0.1499999999999999944, 0.1749999999999999889, 0.2000000000000000111, 0.2250000000000000056, 0.2500000000000000000, 0.2750000000000000222, 0.2999999999999999889, 0.3250000000000000111, 0.3499999999999999778, 0.3750000000000000000, 0.4000000000000000222, 0.4249999999999999889, 0.4500000000000000111, 0.4749999999999999778, 0.5000000000000000000, 0.5250000000000000222, 0.5500000000000000444, 0.5749999999999999556, 0.5999999999999999778, 0.6250000000000000000, 0.6500000000000000222, 0.6750000000000000444, 0.6999999999999999556, 0.7249999999999999778, 0.7500000000000000000, 0.7750000000000000222, 0.8000000000000000444, 0.8249999999999999556, 0.8499999999999999778, 0.8750000000000000000, 0.9000000000000000222, 0.9250000000000000444, 0.9499999999999999556, 0.9749999999999999778, 1.000000000000000000 ),
 .UNSPECIFIED. ) 
 GEOMETRIC_REPRESENTATION_ITEM ( )  RATIONAL_B_SPLINE_SURFACE ( (
 ( 1.000000000000000000, 0.9238795325112867385, 1.000000000000000000, 0.9238795325112867385, 1.000000000000000000, 0.9238795325112867385, 1.000000000000000000, 0.9238795325112867385, 1.000000000000000000, 0.9238795325112867385, 1.000000000000000000, 0.9238795325112867385, 1.000000000000000000, 0.9238795325112867385, 1.000000000000000000, 0.9238795325112867385, 1.000000000000000000, 0.9238795325112867385, 1.000000000000000000, 0.9238795325112867385, 1.000000000000000000, 0.9238795325112867385, 1.000000000000000000, 0.9238795325112867385, 1.000000000000000000, 0.9238795325112867385, 1.000000000000000000, 0.9238795325112867385, 1.000000000000000000, 0.9238795325112867385, 1.000000000000000000, 0.9238795325112867385, 1.000000000000000000, 0.9238795325112867385, 1.000000000000000000, 0.9238795325112867385, 1.000000000000000000, 0.9238795325112867385, 1.000000000000000000, 0.9238795325112867385, 1.000000000000000000, 0.9238795325112867385, 1.000000000000000000, 0.9238795325112867385, 1.000000000000000000, 0.9238795325112867385, 1.000000000000000000, 0.9238795325112867385, 1.000000000000000000, 0.9238795325112867385, 1.000000000000000000, 0.9238795325112867385, 1.000000000000000000, 0.9238795325112867385, 1.000000000000000000, 0.9238795325112867385, 1.000000000000000000, 0.9238795325112867385, 1.000000000000000000, 0.9238795325112867385, 1.000000000000000000, 0.9238795325112867385, 1.000000000000000000, 0.9238795325112867385, 1.000000000000000000, 0.9238795325112867385, 1.000000000000000000, 0.9238795325112867385, 1.000000000000000000, 0.9238795325112867385, 1.000000000000000000, 0.9238795325112867385, 1.000000000000000000, 0.9238795325112867385, 1.000000000000000000, 0.9238795325112867385, 1.000000000000000000, 0.9238795325112867385, 1.000000000000000000, 0.9238795325112867385, 1.000000000000000000),
 ( 1.000000000000000000, 0.9238795325112867385, 1.000000000000000000, 0.9238795325112867385, 1.000000000000000000, 0.9238795325112867385, 1.000000000000000000, 0.9238795325112867385, 1.000000000000000000, 0.9238795325112867385, 1.000000000000000000, 0.9238795325112867385, 1.000000000000000000, 0.9238795325112867385, 1.000000000000000000, 0.9238795325112867385, 1.000000000000000000, 0.9238795325112867385, 1.000000000000000000, 0.9238795325112867385, 1.000000000000000000, 0.9238795325112867385, 1.000000000000000000, 0.9238795325112867385, 1.000000000000000000, 0.9238795325112867385, 1.000000000000000000, 0.9238795325112867385, 1.000000000000000000, 0.9238795325112867385, 1.000000000000000000, 0.9238795325112867385, 1.000000000000000000, 0.9238795325112867385, 1.000000000000000000, 0.9238795325112867385, 1.000000000000000000, 0.9238795325112867385, 1.000000000000000000, 0.9238795325112867385, 1.000000000000000000, 0.9238795325112867385, 1.000000000000000000, 0.9238795325112867385, 1.000000000000000000, 0.9238795325112867385, 1.000000000000000000, 0.9238795325112867385, 1.000000000000000000, 0.9238795325112867385, 1.000000000000000000, 0.9238795325112867385, 1.000000000000000000, 0.9238795325112867385, 1.000000000000000000, 0.9238795325112867385, 1.000000000000000000, 0.9238795325112867385, 1.000000000000000000, 0.9238795325112867385, 1.000000000000000000, 0.9238795325112867385, 1.000000000000000000, 0.9238795325112867385, 1.000000000000000000, 0.9238795325112867385, 1.000000000000000000, 0.9238795325112867385, 1.000000000000000000, 0.9238795325112867385, 1.000000000000000000, 0.9238795325112867385, 1.000000000000000000, 0.9238795325112867385, 1.000000000000000000, 0.9238795325112867385, 1.000000000000000000, 0.9238795325112867385, 1.000000000000000000, 0.9238795325112867385, 1.000000000000000000) ) ) 
 REPRESENTATION_ITEM ( '' )  SURFACE ( )  );
#8221 = EDGE_CURVE ( 'NONE', #2855, #6764, #7114, .T. ) ;
#8222 = CARTESIAN_POINT ( 'NONE',  ( -25.00000000000000000, 5.049999998088170017, -10.35533905932738108 ) ) ;
#8223 = DIRECTION ( 'NONE',  ( 1.000000000000000000, 0.000000000000000000, 0.000000000000000000 ) ) ;
#8224 =( GEOMETRIC_REPRESENTATION_CONTEXT ( 3 ) GLOBAL_UNCERTAINTY_ASSIGNED_CONTEXT ( ( #5715 ) ) GLOBAL_UNIT_ASSIGNED_CONTEXT ( ( #1890, #9565, #6098 ) ) REPRESENTATION_CONTEXT ( 'NONE', 'WORKASPACE' ) );
#8225 = CARTESIAN_POINT ( 'NONE',  ( 1.507608415688466075E-15, 0.4687499990440845421, -24.62111388750000174 ) ) ;
#8226 = DIRECTION ( 'NONE',  ( -0.000000000000000000, 1.000000000000000000, -0.000000000000000000 ) ) ;
#8227 = DIRECTION ( 'NONE',  ( -0.000000000000000000, 1.000000000000000000, -0.000000000000000000 ) ) ;
#8228 = CARTESIAN_POINT ( 'NONE',  ( 1.399999999999998579, 0.000000000000000000, 0.000000000000000000 ) ) ;
#8229 = LINE ( 'NONE', #1552, #3010 ) ;
#8230 = CARTESIAN_POINT ( 'NONE',  ( 29.32100596316561081, 99.46396820659043669, 5.000000000000000000 ) ) ;
#8231 = COLOUR_RGB ( '', 0.40784314, 0.44705882, 0.49803922) ;
#8232 = ORIENTED_EDGE ( 'NONE', *, *, #9839, .T. ) ;
#8233 = ORIENTED_EDGE ( 'NONE', *, *, #10640, .F. ) ;
#8234 = ORIENTED_EDGE ( 'NONE', *, *, #5144, .F. ) ;
#8235 = AXIS2_PLACEMENT_3D ( 'NONE', #9363, #1804, #4345 ) ;
#8236 = UNCERTAINTY_MEASURE_WITH_UNIT (LENGTH_MEASURE( 1.000000000000000082E-05 ), #769, 'distance_accuracy_value', 'NONE');
#8237 = CARTESIAN_POINT ( 'NONE',  ( -10.19839929293505776, 2.531249999044085097, -24.62111388750000174 ) ) ;
#8238 = FACE_OUTER_BOUND ( 'NONE', #1271, .T. ) ;
#8239 = AXIS2_PLACEMENT_3D ( 'NONE', #1875, #10091, #2562 ) ;
#8240 = DIRECTION ( 'NONE',  ( 0.000000000000000000, -0.5150380749100518241, -0.8571673007021137769 ) ) ;
#8241 = DIRECTION ( 'NONE',  ( 2.312964634635745028E-15, 0.000000000000000000, 1.000000000000000000 ) ) ;
#8242 = AXIS2_PLACEMENT_3D ( 'NONE', #1238, #5548, #4572 ) ;
#8243 = CARTESIAN_POINT ( 'NONE',  ( -17.40975659021753330, 1.843749999044084653, 17.40975659021752975 ) ) ;
#8244 = CARTESIAN_POINT ( 'NONE',  ( 0.000000000000000000, 20.00000000000000355, 0.000000000000000000 ) ) ;
#8245 = EDGE_LOOP ( 'NONE', ( #3558, #9678, #6892, #321 ) ) ;
#8246 = VERTEX_POINT ( 'NONE', #6239 ) ;
#8247 = ORIENTED_EDGE ( 'NONE', *, *, #182, .F. ) ;
#8248 = AXIS2_PLACEMENT_3D ( 'NONE', #8576, #4394, #10352 ) ;
#8249 = ORIENTED_EDGE ( 'NONE', *, *, #323, .T. ) ;
#8250 = AXIS2_PLACEMENT_3D ( 'NONE', #10702, #9095, #2303 ) ;
#8251 = CARTESIAN_POINT ( 'NONE',  ( -1.500000000000000444, 83.00000000000000000, 1.499999999999999778 ) ) ;
#8252 = ADVANCED_FACE ( 'NONE', ( #1099 ), #9601, .F. ) ;
#8253 = CARTESIAN_POINT ( 'NONE',  ( 1.135781565508698732E-14, 10.00000000000000355, 12.77350269189627241 ) ) ;
#8254 = DIRECTION ( 'NONE',  ( 0.000000000000000000, 0.000000000000000000, -1.000000000000000000 ) ) ;
#8255 = CARTESIAN_POINT ( 'NONE',  ( -4.592425496802574367E-15, 2.362499998088169129, 25.00000000000000000 ) ) ;
#8256 = LINE ( 'NONE', #4078, #10088 ) ;
#8257 = EDGE_CURVE ( 'NONE', #3818, #417, #6407, .T. ) ;
#8258 = VERTEX_POINT ( 'NONE', #7776 ) ;
#8259 = DIRECTION ( 'NONE',  ( -1.000000000000000000, 0.000000000000000000, -1.047444401652940007E-14 ) ) ;
#8260 = CARTESIAN_POINT ( 'NONE',  ( -10.19839929293505776, 0.7062499990440845865, -24.62111388750000174 ) ) ;
#8261 = ORIENTED_EDGE ( 'NONE', *, *, #2856, .T. ) ;
#8262 = EDGE_CURVE ( 'NONE', #9698, #1394, #5179, .T. ) ;
#8263 = CARTESIAN_POINT ( 'NONE',  ( 6.312177826491054411, 10.00000000000000355, 3.066987298107809679 ) ) ;
#8264 = APPLICATION_PROTOCOL_DEFINITION ( 'draft international standard', 'automotive_design', 1998, #3857 ) ;
#8265 = CARTESIAN_POINT ( 'NONE',  ( 17.67766952966369232, 2.737499998088169573, -17.67766952966369232 ) ) ;
#8266 = ORIENTED_EDGE ( 'NONE', *, *, #3817, .T. ) ;
#8267 = DIRECTION ( 'NONE',  ( 0.1767766952966430272, -0.3535533905932737309, -0.9185586535436907063 ) ) ;
#8268 = CARTESIAN_POINT ( 'NONE',  ( 17.40975659021752620, 1.093749999044084653, 17.40975659021753330 ) ) ;
#8269 = ORIENTED_EDGE ( 'NONE', *, *, #7404, .F. ) ;
#8270 = ADVANCED_FACE ( 'NONE', ( #6900 ), #10256, .F. ) ;
#8271 = EDGE_LOOP ( 'NONE', ( #4406, #5673, #6660, #621 ) ) ;
#8272 = ORIENTED_EDGE ( 'NONE', *, *, #2807, .T. ) ;
#8273 = AXIS2_PLACEMENT_3D ( 'NONE', #4154, #10779, #10893 ) ;
#8274 = AXIS2_PLACEMENT_3D ( 'NONE', #8284, #1718, #10786 ) ;
#8275 = CARTESIAN_POINT ( 'NONE',  ( -25.00000000000000000, 4.049999998088169129, -10.35533905932738108 ) ) ;
#8276 = CARTESIAN_POINT ( 'NONE',  ( 24.62111388749999463, 5.156249999044083765, 10.19839929293507730 ) ) ;
#8277 = CARTESIAN_POINT ( 'NONE',  ( 1.507608415688466075E-15, 3.468749999044085097, -24.62111388750000174 ) ) ;
#8278 = ORIENTED_EDGE ( 'NONE', *, *, #1096, .F. ) ;
#8279 = FACE_OUTER_BOUND ( 'NONE', #3513, .T. ) ;
#8280 = FILL_AREA_STYLE_COLOUR ( '', #4300 ) ;
#8281 = CARTESIAN_POINT ( 'NONE',  ( -25.00000000000001066, 2.174999998088168685, 10.35533905932737397 ) ) ;
#8282 = DIRECTION ( 'NONE',  ( 0.000000000000000000, -2.775557561562888270E-17, -1.000000000000000000 ) ) ;
#8283 = DIRECTION ( 'NONE',  ( 0.000000000000000000, -0.000000000000000000, 1.000000000000000000 ) ) ;
#8284 = CARTESIAN_POINT ( 'NONE',  ( 2.500000000000000444, 1.000000000000002220, -0.5773502691896270633 ) ) ;
#8285 = VECTOR ( 'NONE', #10382, 1000.000000000000000 ) ;
#8286 = VECTOR ( 'NONE', #5747, 1000.000000000000114 ) ;
#8287 = EDGE_CURVE ( 'NONE', #9951, #120, #402, .T. ) ;
#8288 = VERTEX_POINT ( 'NONE', #10689 ) ;
#8289 = ORIENTED_EDGE ( 'NONE', *, *, #119, .F. ) ;
#8290 = ORIENTED_EDGE ( 'NONE', *, *, #10707, .F. ) ;
#8291 = VERTEX_POINT ( 'NONE', #3794 ) ;
#8292 = CIRCLE ( 'NONE', #6539, 4.999999999999997335 ) ;
#8293 = VECTOR ( 'NONE', #3168, 1000.000000000000000 ) ;
#8294 = CARTESIAN_POINT ( 'NONE',  ( -24.62111388750000884, 0.9562499990440846975, 10.19839929293505421 ) ) ;
#8295 = DIRECTION ( 'NONE',  ( -0.000000000000000000, 1.000000000000000000, -0.000000000000000000 ) ) ;
#8296 = CARTESIAN_POINT ( 'NONE',  ( 1.564302918553086774E-15, 7.000000000000003553, -12.77350269189627063 ) ) ;
#8297 = ORIENTED_EDGE ( 'NONE', *, *, #9964, .T. ) ;
#8298 = DIRECTION ( 'NONE',  ( 0.2500000000000009992, -0.8660254037844380415, -0.4330127018922199089 ) ) ;
#8299 = CARTESIAN_POINT ( 'NONE',  ( 1.530808498934191521E-15, 3.862499998088169573, -25.00000000000000000 ) ) ;
#8300 = ADVANCED_FACE ( 'NONE', ( #2939 ), #1402, .T. ) ;
#8301 = CARTESIAN_POINT ( 'NONE',  ( 17.40975659021752620, 3.093749999044084653, 17.40975659021753330 ) ) ;
#8302 = CARTESIAN_POINT ( 'NONE',  ( 15.13990010960492505, -0.001000000000001000089, 5.276923788646651126 ) ) ;
#8303 = ORIENTED_EDGE ( 'NONE', *, *, #2138, .T. ) ;
#8304 = ORIENTED_EDGE ( 'NONE', *, *, #1320, .T. ) ;
#8305 = ORIENTED_EDGE ( 'NONE', *, *, #2943, .T. ) ;
#8306 = CIRCLE ( 'NONE', #4807, 25.00000000000000000 ) ;
#8307 = ORIENTED_EDGE ( 'NONE', *, *, #916, .F. ) ;
#8308 = CYLINDRICAL_SURFACE ( 'NONE', #9743, 5.000000000000000000 ) ;
#8309 = CARTESIAN_POINT ( 'NONE',  ( -6.982120021884473005, 19.03096903053431888, 0.4999999999999268363 ) ) ;
#8310 = DIRECTION ( 'NONE',  ( 0.000000000000000000, 0.000000000000000000, 1.000000000000000000 ) ) ;
#8311 = AXIS2_PLACEMENT_3D ( 'NONE', #9660, #62, #174 ) ;
#8312 = DIRECTION ( 'NONE',  ( 0.000000000000000000, 1.000000000000000000, 0.000000000000000000 ) ) ;
#8313 = CARTESIAN_POINT ( 'NONE',  ( 9.644816411522782573, 5.000000000000000000, 22.72594373997417705 ) ) ;
#8314 = CIRCLE ( 'NONE', #7808, 7.400000000000007461 ) ;
#8315 = PRODUCT_DEFINITION ( 'UNKNOWN', '', #5463, #4055 ) ;
#8316 = ORIENTED_EDGE ( 'NONE', *, *, #6854, .T. ) ;
#8317 = ORIENTED_EDGE ( 'NONE', *, *, #778, .T. ) ;
#8318 = CIRCLE ( 'NONE', #3022, 6.999999999999997335 ) ;
#8319 = DIRECTION ( 'NONE',  ( 0.000000000000000000, -1.000000000000000000, 0.000000000000000000 ) ) ;
#8320 = CYLINDRICAL_SURFACE ( 'NONE', #5834, 2.999999999999999112 ) ;
#8321 = CARTESIAN_POINT ( 'NONE',  ( 10.47307621135324496, 25.00000000000000000, -12.13990010960497479 ) ) ;
#8322 = EDGE_LOOP ( 'NONE', ( #3797, #9643, #10655 ) ) ;
#8323 = AXIS2_PLACEMENT_3D ( 'NONE', #2350, #9191, #5730 ) ;
#8324 = CARTESIAN_POINT ( 'NONE',  ( 10.35533905932737930, 3.799999998088170461, -25.00000000000000000 ) ) ;
#8325 = CARTESIAN_POINT ( 'NONE',  ( 0.000000000000000000, 0.000000000000000000, 0.000000000000000000 ) ) ;
#8326 = VECTOR ( 'NONE', #1562, 1000.000000000000000 ) ;
#8327 = CARTESIAN_POINT ( 'NONE',  ( -3.924072712834378862, 19.03096903053431888, -5.796693311223959810 ) ) ;
#8328 = CARTESIAN_POINT ( 'NONE',  ( -6.062177826491104149, 20.00000000000000355, 3.499999999999936495 ) ) ;
#8329 = CARTESIAN_POINT ( 'NONE',  ( -17.40975659021753330, 0.8437499990440846531, 17.40975659021752975 ) ) ;
#8330 = AXIS2_PLACEMENT_3D ( 'NONE', #3313, #4064, #6658 ) ;
#8331 = ORIENTED_EDGE ( 'NONE', *, *, #1147, .T. ) ;
#8332 = EDGE_CURVE ( 'NONE', #7707, #4862, #9695, .T. ) ;
#8333 = AXIS2_PLACEMENT_3D ( 'NONE', #8446, #9395, #10115 ) ;
#8334 = ORIENTED_EDGE ( 'NONE', *, *, #7539, .T. ) ;
#8335 = EDGE_CURVE ( 'NONE', #2855, #8771, #8146, .T. ) ;
#8336 = CIRCLE ( 'NONE', #3583, 5.000000000000000000 ) ;
#8337 = CARTESIAN_POINT ( 'NONE',  ( 1.530808498934191521E-15, 3.862499998088169573, -25.00000000000000000 ) ) ;
#8338 = DIRECTION ( 'NONE',  ( 0.8660254037844398178, 0.000000000000000000, 0.4999999999999977796 ) ) ;
#8339 = CARTESIAN_POINT ( 'NONE',  ( 24.62111388750000174, 0.2187499990440845699, 0.000000000000000000 ) ) ;
#8340 = CYLINDRICAL_SURFACE ( 'NONE', #2147, 4.999999999999999112 ) ;
#8341 = ORIENTED_EDGE ( 'NONE', *, *, #10388, .T. ) ;
#8342 = CARTESIAN_POINT ( 'NONE',  ( 0.000000000000000000, 28.00000000000000000, 0.000000000000000000 ) ) ;
#8343 =( NAMED_UNIT ( * ) SI_UNIT ( $, .STERADIAN. ) SOLID_ANGLE_UNIT ( ) );
#8344 = EDGE_CURVE ( 'NONE', #7557, #5770, #10738, .T. ) ;
#8345 = DIRECTION ( 'NONE',  ( 0.000000000000000000, 0.000000000000000000, 1.000000000000000000 ) ) ;
#8346 = CARTESIAN_POINT ( 'NONE',  ( -6.223805082245770670, 19.34316356887881483, 3.208128317448866618 ) ) ;
#8347 = CIRCLE ( 'NONE', #3588, 22.00000000000000355 ) ;
#8348 = CARTESIAN_POINT ( 'NONE',  ( 3.924072712834460575, 10.00000000000000355, -5.796693311223904743 ) ) ;
#8349 = CARTESIAN_POINT ( 'NONE',  ( -5.276923788646812774, 28.00000000000000000, -15.13990010960486821 ) ) ;
#8350 = AXIS2_PLACEMENT_3D ( 'NONE', #9090, #3970, #9707 ) ;
#8351 = EDGE_LOOP ( 'NONE', ( #8454, #7470 ) ) ;
#8352 = EDGE_CURVE ( 'NONE', #7304, #5695, #1608, .T. ) ;
#8353 = ORIENTED_EDGE ( 'NONE', *, *, #7467, .T. ) ;
#8354 = VERTEX_POINT ( 'NONE', #8973 ) ;
#8355 = CIRCLE ( 'NONE', #9422, 2.000000000000004441 ) ;
#8356 = UNCERTAINTY_MEASURE_WITH_UNIT (LENGTH_MEASURE( 1.000000000000000082E-05 ), #6637, 'distance_accuracy_value', 'NONE');
#8357 = CARTESIAN_POINT ( 'NONE',  ( -25.00000000000001421, 5.174999998088170017, 10.35533905932737397 ) ) ;
#8358 = CARTESIAN_POINT ( 'NONE',  ( -17.40975659021752975, 0.5937499990440846531, -17.40975659021752975 ) ) ;
#8359 = EDGE_CURVE ( 'NONE', #1133, #10248, #6390, .T. ) ;
#8360 = CARTESIAN_POINT ( 'NONE',  ( 0.000000000000000000, -58.00000000000000000, -24.91176187412963117 ) ) ;
#8361 = DIRECTION ( 'NONE',  ( 0.000000000000000000, -1.000000000000000000, 0.000000000000000000 ) ) ;
#8362 = DIRECTION ( 'NONE',  ( 0.000000000000000000, -1.000000000000000000, 0.000000000000000000 ) ) ;
#8363 = CARTESIAN_POINT ( 'NONE',  ( 17.40975659021752975, 2.343749999044085097, -17.40975659021752975 ) ) ;
#8364 = CARTESIAN_POINT ( 'NONE',  ( -0.5000000000000000000, 0.000000000000000000, 0.000000000000000000 ) ) ;
#8365 = ORIENTED_EDGE ( 'NONE', *, *, #2129, .F. ) ;
#8366 = EDGE_LOOP ( 'NONE', ( #4999, #6663, #5472, #3023 ) ) ;
#8367 = ORIENTED_EDGE ( 'NONE', *, *, #7163, .T. ) ;
#8368 = ORIENTED_EDGE ( 'NONE', *, *, #4138, .F. ) ;
#8369 = ORIENTED_EDGE ( 'NONE', *, *, #3903, .T. ) ;
#8370 = ORIENTED_EDGE ( 'NONE', *, *, #10640, .T. ) ;
#8371 = DIRECTION ( 'NONE',  ( 0.000000000000000000, 0.000000000000000000, 1.000000000000000000 ) ) ;
#8372 = LINE ( 'NONE', #8421, #3952 ) ;
#8373 = CARTESIAN_POINT ( 'NONE',  ( 0.000000000000000000, 10.00000000000000355, 0.000000000000000000 ) ) ;
#8374 = CARTESIAN_POINT ( 'NONE',  ( 11.92163336986831723, 7.781088913245557848, -6.305607966083837113 ) ) ;
#8375 = LINE ( 'NONE', #2616, #7990 ) ;
#8376 = ORIENTED_EDGE ( 'NONE', *, *, #1434, .T. ) ;
#8377 = CARTESIAN_POINT ( 'NONE',  ( -6.296693311223874545, 10.00000000000000355, -3.058047309050087925 ) ) ;
#8378 = DIRECTION ( 'NONE',  ( 0.9185586535436894851, -0.3535533905932744525, 0.1767766952966480787 ) ) ;
#8379 = VERTEX_POINT ( 'NONE', #3842 ) ;
#8380 = DIRECTION ( 'NONE',  ( -1.000000000000000000, 0.000000000000000000, 2.168404344971010347E-16 ) ) ;
#8381 = APPLICATION_PROTOCOL_DEFINITION ( 'draft international standard', 'automotive_design', 1998, #8579 ) ;
#8382 = DIRECTION ( 'NONE',  ( -0.000000000000000000, 1.000000000000000000, 0.000000000000000000 ) ) ;
#8383 = LINE ( 'NONE', #1590, #7122 ) ;
#8384 = CARTESIAN_POINT ( 'NONE',  ( 24.62111388750000174, 3.281249999044084653, -10.19839929293505776 ) ) ;
#8385 = ORIENTED_EDGE ( 'NONE', *, *, #6654, .T. ) ;
#8386 = ORIENTED_EDGE ( 'NONE', *, *, #8828, .F. ) ;
#8387 = DIRECTION ( 'NONE',  ( -0.000000000000000000, -1.000000000000000000, -0.000000000000000000 ) ) ;
#8388 = CARTESIAN_POINT ( 'NONE',  ( 1.507608415688466075E-15, 2.468749999044085097, -24.62111388750000174 ) ) ;
#8389 = FACE_OUTER_BOUND ( 'NONE', #8055, .T. ) ;
#8390 = EDGE_LOOP ( 'NONE', ( #2662, #767, #4703, #1076, #989 ) ) ;
#8391 = PLANE ( 'NONE',  #178 ) ;
#8392 = FACE_OUTER_BOUND ( 'NONE', #10453, .T. ) ;
#8393 = EDGE_CURVE ( 'NONE', #6765, #2700, #9746, .T. ) ;
#8394 = CARTESIAN_POINT ( 'NONE',  ( -0.5590169943749458970, 0.000000000000000000, 0.000000000000000000 ) ) ;
#8395 = DIRECTION ( 'NONE',  ( 0.000000000000000000, -2.775557561562888270E-17, -1.000000000000000000 ) ) ;
#8396 = EDGE_CURVE ( 'NONE', #4628, #2551, #1117, .T. ) ;
#8397 = ORIENTED_EDGE ( 'NONE', *, *, #9822, .T. ) ;
#8398 = VERTEX_POINT ( 'NONE', #3046 ) ;
#8399 = EDGE_LOOP ( 'NONE', ( #7648, #10107 ) ) ;
#8400 = EDGE_CURVE ( 'NONE', #7041, #1422, #1265, .T. ) ;
#8401 = DIRECTION ( 'NONE',  ( -0.000000000000000000, 1.000000000000000000, -0.000000000000000000 ) ) ;
#8402 = CARTESIAN_POINT ( 'NONE',  ( 10.19839929293505953, 0.4062499990440845421, -24.62111388750000174 ) ) ;
#8403 = CARTESIAN_POINT ( 'NONE',  ( 17.67766952966368521, 5.487499998088169129, 17.67766952966369232 ) ) ;
#8404 = CARTESIAN_POINT ( 'NONE',  ( -4.522825247065398226E-15, 1.968749999044084653, 24.62111388750000174 ) ) ;
#8405 = DIRECTION ( 'NONE',  ( 0.000000000000000000, -1.000000000000000000, 0.000000000000000000 ) ) ;
#8406 = ORIENTED_EDGE ( 'NONE', *, *, #2455, .T. ) ;
#8407 = EDGE_CURVE ( 'NONE', #292, #9493, #1252, .T. ) ;
#8408 = DIRECTION ( 'NONE',  ( -0.8660254037844328234, 0.000000000000000000, -0.5000000000000101030 ) ) ;
#8409 = CARTESIAN_POINT ( 'NONE',  ( 0.3335819196118727237, 19.34316356887877930, 6.994037468151971026 ) ) ;
#8410 =( GEOMETRIC_REPRESENTATION_CONTEXT ( 3 ) GLOBAL_UNCERTAINTY_ASSIGNED_CONTEXT ( ( #1725 ) ) GLOBAL_UNIT_ASSIGNED_CONTEXT ( ( #9113, #1712, #8343 ) ) REPRESENTATION_CONTEXT ( 'NONE', 'WORKASPACE' ) );
#8411 = CARTESIAN_POINT ( 'NONE',  ( -17.40975659021753330, 3.843749999044085097, 17.40975659021752975 ) ) ;
#8412 = CARTESIAN_POINT ( 'NONE',  ( -1.400000000000001910, 7.661233032048583711E-16, 5.100000000000006750 ) ) ;
#8413 = ORIENTED_EDGE ( 'NONE', *, *, #6949, .T. ) ;
#8414 = VERTEX_POINT ( 'NONE', #6491 ) ;
#8415 = ORIENTED_EDGE ( 'NONE', *, *, #2418, .F. ) ;
#8416 = EDGE_CURVE ( 'NONE', #8771, #4628, #4634, .T. ) ;
#8417 = EDGE_LOOP ( 'NONE', ( #5587, #550, #9796, #10203 ) ) ;
#8418 = CIRCLE ( 'NONE', #6143, 5.000000000000004441 ) ;
#8419 = AXIS2_PLACEMENT_3D ( 'NONE', #6174, #3562, #5187 ) ;
#8420 = FACE_OUTER_BOUND ( 'NONE', #8322, .T. ) ;
#8421 = CARTESIAN_POINT ( 'NONE',  ( -2.999999999999996447, -0.001000000000001000089, 19.75000000000000000 ) ) ;
#8422 = FACE_OUTER_BOUND ( 'NONE', #3264, .T. ) ;
#8423 = DIRECTION ( 'NONE',  ( 0.000000000000000000, -0.000000000000000000, 1.000000000000000000 ) ) ;
#8424 = CARTESIAN_POINT ( 'NONE',  ( 2.500000000000000444, -1.000000000000003109, 1.732050807568882078 ) ) ;
#8425 = VECTOR ( 'NONE', #9901, 1000.000000000000000 ) ;
#8426 = EDGE_CURVE ( 'NONE', #8118, #4659, #8868, .T. ) ;
#8427 =( REPRESENTATION_RELATIONSHIP ('NONE','NONE', #1269, #7685 ) REPRESENTATION_RELATIONSHIP_WITH_TRANSFORMATION ( #6135 )SHAPE_REPRESENTATION_RELATIONSHIP( ) );
#8428 = ORIENTED_EDGE ( 'NONE', *, *, #7757, .F. ) ;
#8429 = CARTESIAN_POINT ( 'NONE',  ( -19.05903902044739695, 4.999999999999999112, -16.17878337876688022 ) ) ;
#8430 = CARTESIAN_POINT ( 'NONE',  ( -10.35533905932741128, 4.312500000000000888, -24.99999999999996803 ) ) ;
#8431 = CARTESIAN_POINT ( 'NONE',  ( 0.000000000000000000, 28.00000000000000000, 0.000000000000000000 ) ) ;
#8432 = VERTEX_POINT ( 'NONE', #8090 ) ;
#8433 = DIRECTION ( 'NONE',  ( 0.000000000000000000, 1.000000000000000000, 0.000000000000000000 ) ) ;
#8434 = DIRECTION ( 'NONE',  ( 1.000000000000000000, 0.000000000000000000, 0.000000000000000000 ) ) ;
#8435 = CIRCLE ( 'NONE', #1555, 2.999999999999997335 ) ;
#8436 = LINE ( 'NONE', #162, #3935 ) ;
#8437 = FACE_OUTER_BOUND ( 'NONE', #3657, .T. ) ;
#8438 = ORIENTED_EDGE ( 'NONE', *, *, #9356, .T. ) ;
#8439 = CARTESIAN_POINT ( 'NONE',  ( -24.62111388750000174, 1.831249999044084475, -10.19839929293506131 ) ) ;
#8440 = CARTESIAN_POINT ( 'NONE',  ( 1.102066425543451831E-14, 90.00000000000001421, 4.999999999999987566 ) ) ;
#8441 = CARTESIAN_POINT ( 'NONE',  ( -10.19839929293507552, 4.906249999044083765, 24.62111388749999463 ) ) ;
#8442 = FACE_OUTER_BOUND ( 'NONE', #1072, .T. ) ;
#8443 = ORIENTED_EDGE ( 'NONE', *, *, #931, .F. ) ;
#8444 = AXIS2_PLACEMENT_3D ( 'NONE', #3172, #605, #2249 ) ;
#8445 = DIRECTION ( 'NONE',  ( 0.000000000000000000, -1.000000000000000000, 0.000000000000000000 ) ) ;
#8446 = CARTESIAN_POINT ( 'NONE',  ( 0.000000000000000000, 85.00000000000000000, 0.000000000000000000 ) ) ;
#8447 = DIRECTION ( 'NONE',  ( 0.000000000000000000, 1.000000000000000000, 0.000000000000000000 ) ) ;
#8448 = FACE_OUTER_BOUND ( 'NONE', #6611, .T. ) ;
#8449 = FACE_OUTER_BOUND ( 'NONE', #705, .T. ) ;
#8450 = VECTOR ( 'NONE', #6862, 1000.000000000000000 ) ;
#8451 = VECTOR ( 'NONE', #2437, 1000.000000000000000 ) ;
#8452 = ORIENTED_EDGE ( 'NONE', *, *, #4329, .T. ) ;
#8453 = EDGE_LOOP ( 'NONE', ( #3617, #1601, #3143, #505 ) ) ;
#8454 = ORIENTED_EDGE ( 'NONE', *, *, #6411, .T. ) ;
#8455 = ADVANCED_FACE ( 'NONE', ( #424 ), #10528, .F. ) ;
#8456 = DIRECTION ( 'NONE',  ( 1.000000000000000000, 0.000000000000000000, 0.000000000000000000 ) ) ;
#8457 = CARTESIAN_POINT ( 'NONE',  ( 17.40975659021752620, 2.268749999044084475, 17.40975659021753330 ) ) ;
#8458 = CARTESIAN_POINT ( 'NONE',  ( -10.19839929293507552, 3.906249999044085097, 24.62111388749999463 ) ) ;
#8459 =( NAMED_UNIT ( * ) PLANE_ANGLE_UNIT ( ) SI_UNIT ( $, .RADIAN. ) );
#8460 = AXIS2_PLACEMENT_3D ( 'NONE', #10934, #1701, #6738 ) ;
#8461 = AXIS2_PLACEMENT_3D ( 'NONE', #610, #4928, #2212 ) ;
#8462 = EDGE_LOOP ( 'NONE', ( #8818, #6762, #4940 ) ) ;
#8463 = DIRECTION ( 'NONE',  ( 0.000000000000000000, 0.000000000000000000, -1.000000000000000000 ) ) ;
#8464 = ADVANCED_FACE ( 'NONE', ( #5667 ), #2184, .T. ) ;
#8465 = CARTESIAN_POINT ( 'NONE',  ( 0.000000000000000000, 85.00000000000000000, 0.000000000000000000 ) ) ;
#8466 = CARTESIAN_POINT ( 'NONE',  ( 17.67766952966369232, 0.1249999999999999722, -17.67766952966369232 ) ) ;
#8467 = ORIENTED_EDGE ( 'NONE', *, *, #4982, .T. ) ;
#8468 = ORIENTED_EDGE ( 'NONE', *, *, #9227, .T. ) ;
#8469 = ORIENTED_EDGE ( 'NONE', *, *, #6280, .F. ) ;
#8470 = EDGE_LOOP ( 'NONE', ( #4667, #3876, #7913, #6551 ) ) ;
#8471 = AXIS2_PLACEMENT_3D ( 'NONE', #1234, #1290, #9577 ) ;
#8472 =( GEOMETRIC_REPRESENTATION_CONTEXT ( 3 ) GLOBAL_UNCERTAINTY_ASSIGNED_CONTEXT ( ( #70 ) ) GLOBAL_UNIT_ASSIGNED_CONTEXT ( ( #3920, #2243, #1420 ) ) REPRESENTATION_CONTEXT ( 'NONE', 'WORKASPACE' ) );
#8473 = EDGE_CURVE ( 'NONE', #6423, #9073, #9027, .T. ) ;
#8474 = ADVANCED_FACE ( 'NONE', ( #8195 ), #627, .T. ) ;
#8475 = CARTESIAN_POINT ( 'NONE',  ( -7.874999999999821476, 25.00000000000000000, 13.63990010960501031 ) ) ;
#8476 = DIRECTION ( 'NONE',  ( 0.000000000000000000, 1.000000000000000000, 0.000000000000000000 ) ) ;
#8477 = ORIENTED_EDGE ( 'NONE', *, *, #7890, .T. ) ;
#8478 = DIRECTION ( 'NONE',  ( 0.000000000000000000, 1.000000000000000000, 0.000000000000000000 ) ) ;
#8479 = EDGE_CURVE ( 'NONE', #7375, #4001, #4630, .T. ) ;
#8480 = AXIS2_PLACEMENT_3D ( 'NONE', #170, #9515, #1009 ) ;
#8481 = CARTESIAN_POINT ( 'NONE',  ( 25.10306914047445659, 102.1838626489802380, 5.000000000000000000 ) ) ;
#8482 = CARTESIAN_POINT ( 'NONE',  ( 2.999999999999996447, -0.001000000000001000089, -19.75000000000000000 ) ) ;
#8483 = CARTESIAN_POINT ( 'NONE',  ( 24.62111388750000174, 0.3937499990440845310, 0.000000000000000000 ) ) ;
#8484 = EDGE_CURVE ( 'NONE', #1515, #4439, #3338, .T. ) ;
#8485 = ORIENTED_EDGE ( 'NONE', *, *, #10728, .T. ) ;
#8486 = CARTESIAN_POINT ( 'NONE',  ( 0.000000000000000000, 88.00000000000001421, 0.000000000000000000 ) ) ;
#8487 = CARTESIAN_POINT ( 'NONE',  ( 0.000000000000000000, -1.000000000000003331, 0.5773502691896272854 ) ) ;
#8488 = TOROIDAL_SURFACE ( 'NONE', #8845, 6.250000000000000000, 0.7500000000000000000 ) ;
#8489 = CARTESIAN_POINT ( 'NONE',  ( -0.5000000000000000000, 19.03096903053429756, 6.982120021884467675 ) ) ;
#8490 = FACE_OUTER_BOUND ( 'NONE', #1244, .T. ) ;
#8491 = APPLICATION_PROTOCOL_DEFINITION ( 'draft international standard', 'automotive_design', 1998, #4435 ) ;
#8492 = EDGE_CURVE ( 'NONE', #9493, #10743, #10072, .T. ) ;
#8493 = DIRECTION ( 'NONE',  ( 1.000000000000000000, 0.000000000000000000, 0.000000000000000000 ) ) ;
#8494 = DIRECTION ( 'NONE',  ( 1.000000000000000000, 0.000000000000000000, 0.000000000000000000 ) ) ;
#8495 = CARTESIAN_POINT ( 'NONE',  ( -4.522825247065398226E-15, 4.968749999044083765, 24.62111388750000174 ) ) ;
#8496 = AXIS2_PLACEMENT_3D ( 'NONE', #6481, #9837, #7248 ) ;
#8497 = AXIS2_PLACEMENT_3D ( 'NONE', #4959, #6554, #1690 ) ;
#8498 = CARTESIAN_POINT ( 'NONE',  ( 17.40975659021752975, 1.518749999044084698, -17.40975659021752975 ) ) ;
#8499 = CARTESIAN_POINT ( 'NONE',  ( -1.400000000000001910, 0.000000000000000000, 0.000000000000000000 ) ) ;
#8500 = CARTESIAN_POINT ( 'NONE',  ( 17.67766952966368521, 2.875000000000000000, 17.67766952966369232 ) ) ;
#8501 = FACE_OUTER_BOUND ( 'NONE', #5364, .T. ) ;
#8502 = VERTEX_POINT ( 'NONE', #9289 ) ;
#8503 = CYLINDRICAL_SURFACE ( 'NONE', #7094, 2.999999999999997335 ) ;
#8504 = SHAPE_REPRESENTATION_RELATIONSHIP ( 'NONE' , 'NONE' ,  #4232, #5075 ) ;
#8505 = DIRECTION ( 'NONE',  ( 0.000000000000000000, 1.000000000000000000, 0.000000000000000000 ) ) ;
#8506 = CARTESIAN_POINT ( 'NONE',  ( -10.35533905932737575, 1.924999998088169129, -25.00000000000000000 ) ) ;
#8507 = DIRECTION ( 'NONE',  ( 0.000000000000000000, 0.000000000000000000, 1.000000000000000000 ) ) ;
#8508 = CARTESIAN_POINT ( 'NONE',  ( 25.00000000000000000, 4.000000000000000000, 0.000000000000000000 ) ) ;
#8509 = AXIS2_PLACEMENT_3D ( 'NONE', #4534, #3680, #2835 ) ;
#8510 = CIRCLE ( 'NONE', #1825, 5.000000000000004441 ) ;
#8511 = ORIENTED_EDGE ( 'NONE', *, *, #9143, .T. ) ;
#8512 = VERTEX_POINT ( 'NONE', #13 ) ;
#8513 = VERTEX_POINT ( 'NONE', #1508 ) ;
#8514 = VECTOR ( 'NONE', #9132, 1000.000000000000000 ) ;
#8515 = DIRECTION ( 'NONE',  ( 0.000000000000000000, 0.000000000000000000, -1.000000000000000000 ) ) ;
#8516 = CARTESIAN_POINT ( 'NONE',  ( 10.19839929293506486, 4.206249999044085364, 24.62111388749999819 ) ) ;
#8517 = CARTESIAN_POINT ( 'NONE',  ( 10.19839929293505953, 0.5812499990440845865, -24.62111388750000174 ) ) ;
#8518 =( BOUNDED_CURVE ( )  B_SPLINE_CURVE ( 3, ( #159, #3519, #2688, #5258 ),
 .UNSPECIFIED., .F., .F. ) 
 B_SPLINE_CURVE_WITH_KNOTS ( ( 4, 4 ),
 ( 2.284520705739655710, 2.356010155625175795 ),
 .UNSPECIFIED. ) 
 CURVE ( )  GEOMETRIC_REPRESENTATION_ITEM ( )  RATIONAL_B_SPLINE_CURVE ( ( 1.000000000000000000, 0.9995741502243209453, 0.9995741502243209453, 1.000000000000000000 ) ) 
 REPRESENTATION_ITEM ( '' )  );
#8519 = CARTESIAN_POINT ( 'NONE',  ( -4.592425496802574367E-15, 5.362499998088169129, 25.00000000000000000 ) ) ;
#8520 = AXIS2_PLACEMENT_3D ( 'NONE', #10578, #2990, #519 ) ;
#8521 = CARTESIAN_POINT ( 'NONE',  ( 1.530808498934191521E-15, 1.250000000000000000, -25.00000000000000000 ) ) ;
#8522 = SURFACE_STYLE_FILL_AREA ( #5172 ) ;
#8523 = ORIENTED_EDGE ( 'NONE', *, *, #921, .T. ) ;
#8524 = CARTESIAN_POINT ( 'NONE',  ( -11.92163336986836875, 7.781088913245563177, 6.305607966083758953 ) ) ;
#8525 = FACE_BOUND ( 'NONE', #10360, .T. ) ;
#8526 = DIRECTION ( 'NONE',  ( -0.000000000000000000, -1.000000000000000000, -0.000000000000000000 ) ) ;
#8527 = AXIS2_PLACEMENT_3D ( 'NONE', #6625, #999, #5142 ) ;
#8528 = CARTESIAN_POINT ( 'NONE',  ( 25.00000000000000000, 1.000000000000000000, 0.000000000000000000 ) ) ;
#8529 = CARTESIAN_POINT ( 'NONE',  ( -6.776463540776843431, 10.00000000000000355, 7.211537444790383056 ) ) ;
#8530 = ORIENTED_EDGE ( 'NONE', *, *, #1407, .F. ) ;
#8531 = ORIENTED_EDGE ( 'NONE', *, *, #5837, .F. ) ;
#8532 = ORIENTED_EDGE ( 'NONE', *, *, #9761, .F. ) ;
#8533 = ORIENTED_EDGE ( 'NONE', *, *, #1442, .T. ) ;
#8534 = DIRECTION ( 'NONE',  ( -0.8660254037844432595, 0.000000000000000000, 0.4999999999999919509 ) ) ;
#8535 = PLANE ( 'NONE',  #6245 ) ;
#8536 = CARTESIAN_POINT ( 'NONE',  ( 3.957930336368489021E-15, 28.00000000000000000, 22.75000000000000000 ) ) ;
#8537 = DIRECTION ( 'NONE',  ( -0.000000000000000000, 1.000000000000000000, -0.000000000000000000 ) ) ;
#8538 = EDGE_CURVE ( 'NONE', #8662, #2067, #5497, .T. ) ;
#8539 = CYLINDRICAL_SURFACE ( 'NONE', #2014, 25.00000000000000000 ) ;
#8540 = EDGE_CURVE ( 'NONE', #5295, #10359, #1986, .T. ) ;
#8541 = LINE ( 'NONE', #4298, #2457 ) ;
#8542 = CARTESIAN_POINT ( 'NONE',  ( 22.35845142874864422, 5.000000000000000000, 10.92382174880114754 ) ) ;
#8543 = EDGE_CURVE ( 'NONE', #5353, #5479, #2487, .T. ) ;
#8544 = ADVANCED_FACE ( 'NONE', ( #3256 ), #5063, .T. ) ;
#8545 = ORIENTED_EDGE ( 'NONE', *, *, #9107, .T. ) ;
#8546 =( NAMED_UNIT ( * ) PLANE_ANGLE_UNIT ( ) SI_UNIT ( $, .RADIAN. ) );
#8547 = DIRECTION ( 'NONE',  ( 1.156482317317872514E-15, 0.000000000000000000, 1.000000000000000000 ) ) ;
#8548 = CARTESIAN_POINT ( 'NONE',  ( 1.507608415688466075E-15, 2.643749999044084920, -24.62111388750000174 ) ) ;
#8549 = ORIENTED_EDGE ( 'NONE', *, *, #3463, .F. ) ;
#8550 = DIRECTION ( 'NONE',  ( 0.000000000000000000, 1.000000000000000000, 0.000000000000000000 ) ) ;
#8551 = CARTESIAN_POINT ( 'NONE',  ( -20.63749999999999929, -1.387778780781445676E-16, -5.000000000000005329 ) ) ;
#8552 = CARTESIAN_POINT ( 'NONE',  ( -25.00000000000000000, 5.049999998088170017, -10.35533905932738108 ) ) ;
#8553 = EDGE_CURVE ( 'NONE', #5726, #4087, #5822, .T. ) ;
#8554 = CARTESIAN_POINT ( 'NONE',  ( 10.19839929293505953, 4.406249999044084653, -24.62111388750000174 ) ) ;
#8555 = EDGE_CURVE ( 'NONE', #1673, #1427, #3739, .T. ) ;
#8556 = CARTESIAN_POINT ( 'NONE',  ( 10.19839929293505953, 2.581249999044084475, -24.62111388750000174 ) ) ;
#8557 = FACE_OUTER_BOUND ( 'NONE', #3763, .T. ) ;
#8558 = CARTESIAN_POINT ( 'NONE',  ( 25.00000000000000000, 3.000000000000000000, 0.000000000000000000 ) ) ;
#8559 = FACE_OUTER_BOUND ( 'NONE', #4341, .T. ) ;
#8560 = EDGE_LOOP ( 'NONE', ( #487, #8152, #1583, #7358 ) ) ;
#8561 = CARTESIAN_POINT ( 'NONE',  ( -17.67766952966368876, 3.375000000000000000, -17.67766952966369232 ) ) ;
#8562 = FILL_AREA_STYLE_COLOUR ( '', #4564 ) ;
#8563 = DIRECTION ( 'NONE',  ( 0.000000000000000000, 1.000000000000000000, 0.000000000000000000 ) ) ;
#8564 = FACE_BOUND ( 'NONE', #9520, .T. ) ;
#8565 = CARTESIAN_POINT ( 'NONE',  ( -25.00000000000001421, 1.174999998088169351, 10.35533905932737397 ) ) ;
#8566 = LINE ( 'NONE', #6038, #9570 ) ;
#8567 = CARTESIAN_POINT ( 'NONE',  ( -25.00000000000000000, 3.500000000000000000, -3.061616997868383043E-15 ) ) ;
#8568 = VERTEX_POINT ( 'NONE', #8299 ) ;
#8569 = ADVANCED_FACE ( 'NONE', ( #742 ), #5010, .T. ) ;
#8570 = EDGE_LOOP ( 'NONE', ( #5674, #4038, #714, #10079 ) ) ;
#8571 = DIRECTION ( 'NONE',  ( -0.000000000000000000, 1.000000000000000000, -0.000000000000000000 ) ) ;
#8572 = CARTESIAN_POINT ( 'NONE',  ( 17.40975659021752620, 4.268749999044085364, 17.40975659021753330 ) ) ;
#8573 = CARTESIAN_POINT ( 'NONE',  ( 25.52691073765301510, 98.96446609406727646, 5.000000000000000000 ) ) ;
#8574 = CARTESIAN_POINT ( 'NONE',  ( 17.67766952966369232, 2.737499998088169573, -17.67766952966369232 ) ) ;
#8575 = CARTESIAN_POINT ( 'NONE',  ( 25.00000000000000000, -2.710505431213761085E-17, 0.000000000000000000 ) ) ;
#8576 = CARTESIAN_POINT ( 'NONE',  ( 82.32050807568876394, 100.2820323027551268, 0.000000000000000000 ) ) ;
#8577 = LINE ( 'NONE', #7759, #4907 ) ;
#8578 = DIRECTION ( 'NONE',  ( 0.000000000000000000, 0.000000000000000000, -1.000000000000000000 ) ) ;
#8579 = APPLICATION_CONTEXT ( 'automotive_design' ) ;
#8580 = CYLINDRICAL_SURFACE ( 'NONE', #10261, 6.750000000000007994 ) ;
#8581 = FACE_OUTER_BOUND ( 'NONE', #834, .T. ) ;
#8582 = CARTESIAN_POINT ( 'NONE',  ( -17.67766952966368876, 1.375000000000000000, -17.67766952966369232 ) ) ;
#8583 = CARTESIAN_POINT ( 'NONE',  ( 18.60400172474268032, 28.00000000000000000, 7.276923788646641356 ) ) ;
#8584 = ORIENTED_EDGE ( 'NONE', *, *, #439, .F. ) ;
#8585 = VERTEX_POINT ( 'NONE', #10133 ) ;
#8586 = ORIENTED_EDGE ( 'NONE', *, *, #7007, .T. ) ;
#8587 = VERTEX_POINT ( 'NONE', #2545 ) ;
#8588 =( BOUNDED_CURVE ( )  B_SPLINE_CURVE ( 2, ( #3592, #1120, #10338, #166, #889, #9326, #10215, #9266, #5090 ),
 .UNSPECIFIED., .F., .F. ) 
 B_SPLINE_CURVE_WITH_KNOTS ( ( 3, 2, 2, 2, 3 ),
 ( 0.05000000000000000278, 0.07499999999999999722, 0.1000000000000000056, 0.1250000000000000000, 0.1499999999999999944 ),
 .UNSPECIFIED. ) 
 CURVE ( )  GEOMETRIC_REPRESENTATION_ITEM ( )  RATIONAL_B_SPLINE_CURVE ( ( 1.000000000000000000, 0.9238795325112867385, 1.000000000000000000, 0.9238795325112867385, 1.000000000000000000, 0.9238795325112867385, 1.000000000000000000, 0.9238795325112867385, 1.000000000000000000 ) ) 
 REPRESENTATION_ITEM ( '' )  );
#8589 = PRESENTATION_LAYER_ASSIGNMENT (  '', '', ( #8942 ) ) ;
#8590 = CARTESIAN_POINT ( 'NONE',  ( 1.500000000000001332, 0.000000000000000000, 0.000000000000000000 ) ) ;
#8591 = ORIENTED_EDGE ( 'NONE', *, *, #10713, .T. ) ;
#8592 = PLANE ( 'NONE',  #4125 ) ;
#8593 = CARTESIAN_POINT ( 'NONE',  ( -6.062177826491028654, 20.00000000000000355, -3.500000000000069722 ) ) ;
#8594 = DIRECTION ( 'NONE',  ( -1.000000000000000000, 0.000000000000000000, 0.000000000000000000 ) ) ;
#8595 = CARTESIAN_POINT ( 'NONE',  ( 0.000000000000000000, 10.00000000000000355, 0.000000000000000000 ) ) ;
#8596 = CARTESIAN_POINT ( 'NONE',  ( 14.00000000000000533, 0.000000000000000000, 0.000000000000000000 ) ) ;
#8597 = CARTESIAN_POINT ( 'NONE',  ( 17.40975659021752620, 5.268749999044085364, 17.40975659021753330 ) ) ;
#8598 = VECTOR ( 'NONE', #6676, 1000.000000000000000 ) ;
#8599 = EDGE_LOOP ( 'NONE', ( #198, #2800, #7266, #8739 ) ) ;
#8600 = ADVANCED_FACE ( 'NONE', ( #10858 ), #8488, .T. ) ;
#8601 = EDGE_CURVE ( 'NONE', #2611, #2038, #5913, .T. ) ;
#8602 = FACE_OUTER_BOUND ( 'NONE', #3966, .T. ) ;
#8603 = DIRECTION ( 'NONE',  ( 0.000000000000000000, 0.8660254037844385966, 0.5000000000000001110 ) ) ;
#8604 = CARTESIAN_POINT ( 'NONE',  ( -24.62111388750000174, 3.893749999044084475, -3.015216831376932151E-15 ) ) ;
#8605 = ORIENTED_EDGE ( 'NONE', *, *, #9765, .F. ) ;
#8606 = DIRECTION ( 'NONE',  ( 0.000000000000000000, 1.000000000000000000, 0.000000000000000000 ) ) ;
#8607 = DIRECTION ( 'NONE',  ( -0.000000000000000000, 1.000000000000000000, 0.000000000000000000 ) ) ;
#8608 = CARTESIAN_POINT ( 'NONE',  ( 6.062177826491077504, 20.00000000000000355, -3.499999999999985345 ) ) ;
#8609 = CARTESIAN_POINT ( 'NONE',  ( -17.40975659021752975, 3.593749999044084653, -17.40975659021752975 ) ) ;
#8610 = EDGE_CURVE ( 'NONE', #3100, #7830, #6223, .T. ) ;
#8611 = VECTOR ( 'NONE', #10353, 1000.000000000000000 ) ;
#8612 =( GEOMETRIC_REPRESENTATION_CONTEXT ( 3 ) GLOBAL_UNCERTAINTY_ASSIGNED_CONTEXT ( ( #5606 ) ) GLOBAL_UNIT_ASSIGNED_CONTEXT ( ( #352, #6379, #8906 ) ) REPRESENTATION_CONTEXT ( 'NONE', 'WORKASPACE' ) );
#8613 = ADVANCED_FACE ( 'NONE', ( #685 ), #3610, .T. ) ;
#8614 = CARTESIAN_POINT ( 'NONE',  ( 1.507608415688466075E-15, 1.643749999044084475, -24.62111388750000174 ) ) ;
#8615 = CARTESIAN_POINT ( 'NONE',  ( 24.62111388750000174, 1.393749999044084475, 0.000000000000000000 ) ) ;
#8616 = DIRECTION ( 'NONE',  ( -0.8660254037844382635, -0.5000000000000004441, 0.000000000000000000 ) ) ;
#8617 = VECTOR ( 'NONE', #6875, 999.9999999999998863 ) ;
#8618 = FACE_OUTER_BOUND ( 'NONE', #776, .T. ) ;
#8619 = CARTESIAN_POINT ( 'NONE',  ( -24.62111388750000884, 1.956249999044084698, 10.19839929293505421 ) ) ;
#8620 = VERTEX_POINT ( 'NONE', #6998 ) ;
#8621 = CARTESIAN_POINT ( 'NONE',  ( 0.000000000000000000, 82.00000000000000000, 6.000000000000000888 ) ) ;
#8622 = CARTESIAN_POINT ( 'NONE',  ( -0.5000000000000000000, 10.00000000000000355, 6.982120021884467675 ) ) ;
#8623 = DIRECTION ( 'NONE',  ( -0.4330127018922207971, 0.8660254037844380415, 0.2499999999999995282 ) ) ;
#8624 = CARTESIAN_POINT ( 'NONE',  ( 25.00000000000000000, 3.000000000000000000, 0.000000000000000000 ) ) ;
#8625 = ADVANCED_FACE ( 'NONE', ( #6054 ), #8638, .F. ) ;
#8626 = ORIENTED_EDGE ( 'NONE', *, *, #7163, .F. ) ;
#8627 = ORIENTED_EDGE ( 'NONE', *, *, #4721, .T. ) ;
#8628 = FACE_OUTER_BOUND ( 'NONE', #2051, .T. ) ;
#8629 = CARTESIAN_POINT ( 'NONE',  ( -10.19839929293505776, 4.706249999044086252, -24.62111388750000174 ) ) ;
#8630 = LINE ( 'NONE', #8573, #1125 ) ;
#8631 = CARTESIAN_POINT ( 'NONE',  ( 10.35533905932737930, 3.799999998088170017, -25.00000000000000000 ) ) ;
#8632 = CARTESIAN_POINT ( 'NONE',  ( -10.19839929293505776, 4.531249999044084653, -24.62111388750000174 ) ) ;
#8633 = LINE ( 'NONE', #10180, #7366 ) ;
#8634 = ADVANCED_FACE ( 'NONE', ( #10243 ), #4400, .T. ) ;
#8635 = ORIENTED_EDGE ( 'NONE', *, *, #2925, .F. ) ;
#8636 = CARTESIAN_POINT ( 'NONE',  ( 1.102066425543451831E-14, 88.00000000000001421, 4.999999999999987566 ) ) ;
#8637 = FACE_BOUND ( 'NONE', #4012, .T. ) ;
#8638 = CYLINDRICAL_SURFACE ( 'NONE', #3169, 2.999999999999997335 ) ;
#8639 = CARTESIAN_POINT ( 'NONE',  ( -7.276923788646840308, 25.00000000000000000, -18.60400172474260216 ) ) ;
#8640 = ADVANCED_FACE ( 'NONE', ( #9415 ), #8580, .F. ) ;
#8641 = CARTESIAN_POINT ( 'NONE',  ( -24.62111388750000884, 4.781249999044083765, 10.19839929293505421 ) ) ;
#8642 = DIRECTION ( 'NONE',  ( 1.000000000000000000, 0.000000000000000000, 0.000000000000000000 ) ) ;
#8643 = ORIENTED_EDGE ( 'NONE', *, *, #520, .F. ) ;
#8644 = ORIENTED_EDGE ( 'NONE', *, *, #2914, .T. ) ;
#8645 = ORIENTED_EDGE ( 'NONE', *, *, #6352, .T. ) ;
#8646 = PRODUCT_DEFINITION_SHAPE ( 'NONE', 'NONE',  #10953 ) ;
#8647 = ORIENTED_EDGE ( 'NONE', *, *, #10033, .T. ) ;
#8648 = CARTESIAN_POINT ( 'NONE',  ( 0.000000000000000000, 5.000000000000000000, -25.00000000000000000 ) ) ;
#8649 = VECTOR ( 'NONE', #2134, 1000.000000000000000 ) ;
#8650 = AXIS2_PLACEMENT_3D ( 'NONE', #3727, #5288, #10467 ) ;
#8651 = EDGE_CURVE ( 'NONE', #8512, #5101, #1854, .T. ) ;
#8652 = CARTESIAN_POINT ( 'NONE',  ( 24.81055694375000087, 5.109374999522041882, 0.000000000000000000 ) ) ;
#8653 = CARTESIAN_POINT ( 'NONE',  ( 0.1920286436967143240, 0.000000000000000000, 0.000000000000000000 ) ) ;
#8654 = DIRECTION ( 'NONE',  ( 0.8660254037844399289, 0.000000000000000000, 0.4999999999999977796 ) ) ;
#8655 = CARTESIAN_POINT ( 'NONE',  ( 2.143131898507867459E-15, 8.000000000000000000, -15.00000000000000178 ) ) ;
#8656 = CARTESIAN_POINT ( 'NONE',  ( 0.000000000000000000, -55.00000000000000000, 24.91176187412963117 ) ) ;
#8657 = CIRCLE ( 'NONE', #6380, 6.999999999999997335 ) ;
#8658 = VECTOR ( 'NONE', #5647, 1000.000000000000000 ) ;
#8659 =( BOUNDED_SURFACE ( )  B_SPLINE_SURFACE ( 1, 2, ( 
 ( #5491, #510, #2927, #8854, #7199, #1297, #410, #2975, #3784, #2216, #3880, #9012, #4679, #1438, #3996, #4832, #2166, #616, #8029, #6383, #5549, #8908, #10724, #1342, #9526, #6941, #6220, #10350, #2713, #9470, #7875, #6109, #1963, #2021, #8574, #298, #3663, #6162, #7815, #7046, #5336, #248, #6878, #8750, #10404, #1140, #2822, #8694, #4520, #1902, #5283, #8631, #5393, #186, #9581, #10299, #1188, #1080, #1848, #4569, #2651, #10236, #6049, #9408, #5231, #7754, #1023, #4456, #3606, #6994, #2763, #4392, #3546, #8357, #7475, #5002, #8519, #5814, #8403, #4164, #3429 ),
 ( #9124, #10128, #10009, #3305, #9, #10178, #10851, #10905, #5106, #8294, #3249, #7577, #6768, #127, #971, #9233, #9285, #4274, #2596, #2540, #10068, #5990, #4335, #906, #846, #5933, #7526, #4214, #6708, #5059, #7638, #2434, #74, #5758, #6821, #9345, #1789, #5170, #7698, #2483, #3488, #6648, #9178, #9954, #2385, #4943, #5879, #735, #798, #1677, #316, #6967, #1985, #1208, #269, #1924, #152, #10372, #6904, #8769, #10425, #5305, #4354, #1103, #7938, #9547, #10260, #6077, #2785, #4483, #9490, #6181, #6244, #2842, #3572, #5252, #10323, #2037, #8597, #7895, #5361 ) ),
 .UNSPECIFIED., .F., .F., .F. ) 
 B_SPLINE_SURFACE_WITH_KNOTS ( ( 2, 2 ),
 ( 3, 2, 2, 2, 2, 2, 2, 2, 2, 2, 2, 2, 2, 2, 2, 2, 2, 2, 2, 2, 2, 2, 2, 2, 2, 2, 2, 2, 2, 2, 2, 2, 2, 2, 2, 2, 2, 2, 2, 2, 3 ),
 ( 0.000000000000000000, 1.000000000000000000 ),
 ( 0.000000000000000000, 0.02500000000000000139, 0.05000000000000000278, 0.07499999999999999722, 0.1000000000000000056, 0.1250000000000000000, 0.1499999999999999944, 0.1749999999999999889, 0.2000000000000000111, 0.2250000000000000056, 0.2500000000000000000, 0.2750000000000000222, 0.2999999999999999889, 0.3250000000000000111, 0.3499999999999999778, 0.3750000000000000000, 0.4000000000000000222, 0.4249999999999999889, 0.4500000000000000111, 0.4749999999999999778, 0.5000000000000000000, 0.5250000000000000222, 0.5500000000000000444, 0.5749999999999999556, 0.5999999999999999778, 0.6250000000000000000, 0.6500000000000000222, 0.6750000000000000444, 0.6999999999999999556, 0.7249999999999999778, 0.7500000000000000000, 0.7750000000000000222, 0.8000000000000000444, 0.8249999999999999556, 0.8499999999999999778, 0.8750000000000000000, 0.9000000000000000222, 0.9250000000000000444, 0.9499999999999999556, 0.9749999999999999778, 1.000000000000000000 ),
 .UNSPECIFIED. ) 
 GEOMETRIC_REPRESENTATION_ITEM ( )  RATIONAL_B_SPLINE_SURFACE ( (
 ( 1.000000000000000000, 0.9238795325112867385, 1.000000000000000000, 0.9238795325112867385, 1.000000000000000000, 0.9238795325112867385, 1.000000000000000000, 0.9238795325112867385, 1.000000000000000000, 0.9238795325112867385, 1.000000000000000000, 0.9238795325112867385, 1.000000000000000000, 0.9238795325112867385, 1.000000000000000000, 0.9238795325112867385, 1.000000000000000000, 0.9238795325112867385, 1.000000000000000000, 0.9238795325112867385, 1.000000000000000000, 0.9238795325112867385, 1.000000000000000000, 0.9238795325112867385, 1.000000000000000000, 0.9238795325112867385, 1.000000000000000000, 0.9238795325112867385, 1.000000000000000000, 0.9238795325112867385, 1.000000000000000000, 0.9238795325112867385, 1.000000000000000000, 0.9238795325112867385, 1.000000000000000000, 0.9238795325112867385, 1.000000000000000000, 0.9238795325112867385, 1.000000000000000000, 0.9238795325112867385, 1.000000000000000000, 0.9238795325112867385, 1.000000000000000000, 0.9238795325112867385, 1.000000000000000000, 0.9238795325112867385, 1.000000000000000000, 0.9238795325112867385, 1.000000000000000000, 0.9238795325112867385, 1.000000000000000000, 0.9238795325112867385, 1.000000000000000000, 0.9238795325112867385, 1.000000000000000000, 0.9238795325112867385, 1.000000000000000000, 0.9238795325112867385, 1.000000000000000000, 0.9238795325112867385, 1.000000000000000000, 0.9238795325112867385, 1.000000000000000000, 0.9238795325112867385, 1.000000000000000000, 0.9238795325112867385, 1.000000000000000000, 0.9238795325112867385, 1.000000000000000000, 0.9238795325112867385, 1.000000000000000000, 0.9238795325112867385, 1.000000000000000000, 0.9238795325112867385, 1.000000000000000000, 0.9238795325112867385, 1.000000000000000000, 0.9238795325112867385, 1.000000000000000000, 0.9238795325112867385, 1.000000000000000000),
 ( 1.000000000000000000, 0.9238795325112867385, 1.000000000000000000, 0.9238795325112867385, 1.000000000000000000, 0.9238795325112867385, 1.000000000000000000, 0.9238795325112867385, 1.000000000000000000, 0.9238795325112867385, 1.000000000000000000, 0.9238795325112867385, 1.000000000000000000, 0.9238795325112867385, 1.000000000000000000, 0.9238795325112867385, 1.000000000000000000, 0.9238795325112867385, 1.000000000000000000, 0.9238795325112867385, 1.000000000000000000, 0.9238795325112867385, 1.000000000000000000, 0.9238795325112867385, 1.000000000000000000, 0.9238795325112867385, 1.000000000000000000, 0.9238795325112867385, 1.000000000000000000, 0.9238795325112867385, 1.000000000000000000, 0.9238795325112867385, 1.000000000000000000, 0.9238795325112867385, 1.000000000000000000, 0.9238795325112867385, 1.000000000000000000, 0.9238795325112867385, 1.000000000000000000, 0.9238795325112867385, 1.000000000000000000, 0.9238795325112867385, 1.000000000000000000, 0.9238795325112867385, 1.000000000000000000, 0.9238795325112867385, 1.000000000000000000, 0.9238795325112867385, 1.000000000000000000, 0.9238795325112867385, 1.000000000000000000, 0.9238795325112867385, 1.000000000000000000, 0.9238795325112867385, 1.000000000000000000, 0.9238795325112867385, 1.000000000000000000, 0.9238795325112867385, 1.000000000000000000, 0.9238795325112867385, 1.000000000000000000, 0.9238795325112867385, 1.000000000000000000, 0.9238795325112867385, 1.000000000000000000, 0.9238795325112867385, 1.000000000000000000, 0.9238795325112867385, 1.000000000000000000, 0.9238795325112867385, 1.000000000000000000, 0.9238795325112867385, 1.000000000000000000, 0.9238795325112867385, 1.000000000000000000, 0.9238795325112867385, 1.000000000000000000, 0.9238795325112867385, 1.000000000000000000, 0.9238795325112867385, 1.000000000000000000) ) ) 
 REPRESENTATION_ITEM ( '' )  SURFACE ( )  );
#8660 = ORIENTED_EDGE ( 'NONE', *, *, #9085, .F. ) ;
#8661 = ORIENTED_EDGE ( 'NONE', *, *, #261, .T. ) ;
#8662 = VERTEX_POINT ( 'NONE', #7879 ) ;
#8663 = AXIS2_PLACEMENT_3D ( 'NONE', #3496, #9476, #6279 ) ;
#8664 = DIRECTION ( 'NONE',  ( 0.4999999999999967248, 1.060575238724909133E-16, 0.8660254037844404840 ) ) ;
#8665 = CARTESIAN_POINT ( 'NONE',  ( -1.745740669421566678E-15, 0.000000000000000000, 0.5000000000000000000 ) ) ;
#8666 = VECTOR ( 'NONE', #3454, 1000.000000000000000 ) ;
#8667 = CARTESIAN_POINT ( 'NONE',  ( -17.40975659021753330, 1.018749999044084698, 17.40975659021752975 ) ) ;
#8668 = ORIENTED_EDGE ( 'NONE', *, *, #10728, .F. ) ;
#8669 = CARTESIAN_POINT ( 'NONE',  ( 3.957930336368489021E-15, 25.00000000000000000, 22.75000000000000000 ) ) ;
#8670 = CARTESIAN_POINT ( 'NONE',  ( -6.386751345948222358, 10.00000000000000355, 11.06217782649103043 ) ) ;
#8671 = LINE ( 'NONE', #1114, #751 ) ;
#8672 = DIRECTION ( 'NONE',  ( -0.000000000000000000, -1.000000000000000000, -0.000000000000000000 ) ) ;
#8673 = EDGE_LOOP ( 'NONE', ( #858, #4267, #5092, #10075, #5588, #9896 ) ) ;
#8674 = AXIS2_PLACEMENT_3D ( 'NONE', #7104, #2217, #4724 ) ;
#8675 = CARTESIAN_POINT ( 'NONE',  ( 0.000000000000000000, 82.00000000000000000, 0.000000000000000000 ) ) ;
#8676 = DIRECTION ( 'NONE',  ( 1.000000000000000000, 0.000000000000000000, 0.000000000000000000 ) ) ;
#8677 = DIRECTION ( 'NONE',  ( 0.000000000000000000, -1.000000000000000000, 0.000000000000000000 ) ) ;
#8678 = VERTEX_POINT ( 'NONE', #5399 ) ;
#8679 = CARTESIAN_POINT ( 'NONE',  ( 1.499999999999999556, 83.00000000000000000, -1.500000000000000222 ) ) ;
#8680 = DIRECTION ( 'NONE',  ( 0.000000000000000000, -1.000000000000000000, 0.000000000000000000 ) ) ;
#8681 = CARTESIAN_POINT ( 'NONE',  ( 24.62111388750000174, 0.2187499990440845699, 0.000000000000000000 ) ) ;
#8682 = CARTESIAN_POINT ( 'NONE',  ( -4.592425496802574367E-15, 1.362499998088169129, 25.00000000000000000 ) ) ;
#8683 = AXIS2_PLACEMENT_3D ( 'NONE', #2378, #10118, #8283 ) ;
#8684 = EDGE_CURVE ( 'NONE', #3847, #2572, #5160, .T. ) ;
#8685 = EDGE_CURVE ( 'NONE', #5242, #10312, #10185, .T. ) ;
#8686 = ORIENTED_EDGE ( 'NONE', *, *, #7106, .T. ) ;
#8687 = ORIENTED_EDGE ( 'NONE', *, *, #9761, .T. ) ;
#8688 = ORIENTED_EDGE ( 'NONE', *, *, #8947, .F. ) ;
#8689 = EDGE_CURVE ( 'NONE', #528, #3304, #10610, .T. ) ;
#8690 = CARTESIAN_POINT ( 'NONE',  ( 1.499999999999999556, 88.00000000000001421, -1.500000000000000222 ) ) ;
#8691 = CARTESIAN_POINT ( 'NONE',  ( 1.507608415688466075E-15, 1.468749999044084431, -24.62111388750000174 ) ) ;
#8692 = AXIS2_PLACEMENT_3D ( 'NONE', #2077, #6903, #7066 ) ;
#8693 = CARTESIAN_POINT ( 'NONE',  ( 25.00000000000000000, 0.6124999980881691286, 0.000000000000000000 ) ) ;
#8694 = CARTESIAN_POINT ( 'NONE',  ( 24.99999999999999289, 3.549999998088169573, 10.35533905932739529 ) ) ;
#8695 = CARTESIAN_POINT ( 'NONE',  ( -24.62111388750000174, 4.718749999044084653, -3.015216831376932151E-15 ) ) ;
#8696 = VECTOR ( 'NONE', #5945, 999.9999999999998863 ) ;
#8697 = CARTESIAN_POINT ( 'NONE',  ( 10.35640646055104064, 93.66987298107783033, -5.000000000000000000 ) ) ;
#8698 = CARTESIAN_POINT ( 'NONE',  ( 0.000000000000000000, 10.00000000000000355, 0.000000000000000000 ) ) ;
#8699 = AXIS2_PLACEMENT_3D ( 'NONE', #7674, #222, #6137 ) ;
#8700 = DIRECTION ( 'NONE',  ( 8.881784197001254296E-16, 0.000000000000000000, 1.000000000000000000 ) ) ;
#8701 = CARTESIAN_POINT ( 'NONE',  ( -4.592425496802574367E-15, 1.750000000000000000, 25.00000000000000000 ) ) ;
#8702 = ADVANCED_FACE ( 'NONE', ( #1907 ), #6944, .F. ) ;
#8703 = DIRECTION ( 'NONE',  ( -9.251858538542978533E-15, 0.000000000000000000, 1.000000000000000000 ) ) ;
#8704 = ORIENTED_EDGE ( 'NONE', *, *, #797, .T. ) ;
#8705 = AXIS2_PLACEMENT_3D ( 'NONE', #2821, #3428, #5104 ) ;
#8706 = ORIENTED_EDGE ( 'NONE', *, *, #1127, .T. ) ;
#8707 = ORIENTED_EDGE ( 'NONE', *, *, #7018, .F. ) ;
#8708 = ORIENTED_EDGE ( 'NONE', *, *, #6216, .T. ) ;
#8709 = ADVANCED_FACE ( 'NONE', ( #5341 ), #6114, .F. ) ;
#8710 = CIRCLE ( 'NONE', #5880, 2.999999999999996891 ) ;
#8711 = PLANE ( 'NONE',  #2075 ) ;
#8712 = AXIS2_PLACEMENT_3D ( 'NONE', #6299, #1172, #5373 ) ;
#8713 = EDGE_CURVE ( 'NONE', #8678, #5068, #1087, .T. ) ;
#8714 = LINE ( 'NONE', #10315, #10096 ) ;
#8715 = LINE ( 'NONE', #312, #9764 ) ;
#8716 = CARTESIAN_POINT ( 'NONE',  ( 15.60400172474269453, -0.001000000000001000089, 12.47307621135327693 ) ) ;
#8717 = CARTESIAN_POINT ( 'NONE',  ( 6.776463540776787475, 10.00000000000000355, -7.211537444790439899 ) ) ;
#8718 = CARTESIAN_POINT ( 'NONE',  ( 5.999999999999996447, 10.00000000000000355, 0.5000000000000209832 ) ) ;
#8719 = DIRECTION ( 'NONE',  ( -0.000000000000000000, -1.000000000000000000, -0.000000000000000000 ) ) ;
#8720 = DIRECTION ( 'NONE',  ( 0.000000000000000000, 1.000000000000000000, 0.000000000000000000 ) ) ;
#8721 = ORIENTED_EDGE ( 'NONE', *, *, #382, .T. ) ;
#8722 = ORIENTED_EDGE ( 'NONE', *, *, #6350, .T. ) ;
#8723 = CIRCLE ( 'NONE', #7138, 6.999999999999997335 ) ;
#8724 = EDGE_LOOP ( 'NONE', ( #7386, #6562, #7613, #7587 ) ) ;
#8725 = CARTESIAN_POINT ( 'NONE',  ( -4.592425496802574367E-15, 4.750000000000000000, 25.00000000000000000 ) ) ;
#8726 = CARTESIAN_POINT ( 'NONE',  ( 24.99999999999999289, 1.549999998088169129, 10.35533905932739529 ) ) ;
#8727 = CARTESIAN_POINT ( 'NONE',  ( -17.40975659021753330, 3.018749999044084475, 17.40975659021752975 ) ) ;
#8728 = ORIENTED_EDGE ( 'NONE', *, *, #10865, .T. ) ;
#8729 = CYLINDRICAL_SURFACE ( 'NONE', #10300, 25.00000000000000000 ) ;
#8730 = LINE ( 'NONE', #327, #31 ) ;
#8731 =( BOUNDED_CURVE ( )  B_SPLINE_CURVE ( 2, ( #7917, #8944, #2868, #7968, #3769, #10504, #1376, #6265, #4761 ),
 .UNSPECIFIED., .F., .F. ) 
 B_SPLINE_CURVE_WITH_KNOTS ( ( 3, 2, 2, 2, 3 ),
 ( 0.3499999999999999778, 0.3750000000000000000, 0.4000000000000000222, 0.4249999999999999889, 0.4500000000000000111 ),
 .UNSPECIFIED. ) 
 CURVE ( )  GEOMETRIC_REPRESENTATION_ITEM ( )  RATIONAL_B_SPLINE_CURVE ( ( 1.000000000000000000, 0.9238795325112867385, 1.000000000000000000, 0.9238795325112867385, 1.000000000000000000, 0.9238795325112867385, 1.000000000000000000, 0.9238795325112867385, 1.000000000000000000 ) ) 
 REPRESENTATION_ITEM ( '' )  );
#8732 = LINE ( 'NONE', #8004, #3037 ) ;
#8733 = ORIENTED_EDGE ( 'NONE', *, *, #10707, .T. ) ;
#8734 = EDGE_CURVE ( 'NONE', #1424, #10065, #5624, .T. ) ;
#8735 = VERTEX_POINT ( 'NONE', #2600 ) ;
#8736 = DIRECTION ( 'NONE',  ( 1.000000000000000000, 0.000000000000000000, 0.000000000000000000 ) ) ;
#8737 = CARTESIAN_POINT ( 'NONE',  ( -24.26769393075472436, 4.999999999999999112, 5.061130139468667188 ) ) ;
#8738 = CARTESIAN_POINT ( 'NONE',  ( 24.62111388750000174, 1.393749999044084475, 0.000000000000000000 ) ) ;
#8739 = ORIENTED_EDGE ( 'NONE', *, *, #2455, .F. ) ;
#8740 = CARTESIAN_POINT ( 'NONE',  ( 18.60400172474263414, 25.00000000000000000, -7.276923788646775471 ) ) ;
#8741 = CARTESIAN_POINT ( 'NONE',  ( 0.000000000000000000, 25.00000000000000000, -5.999999999999999112 ) ) ;
#8742 = CARTESIAN_POINT ( 'NONE',  ( 17.40975659021752975, 4.343749999044084653, -17.40975659021752975 ) ) ;
#8743 = DIRECTION ( 'NONE',  ( 0.000000000000000000, 0.000000000000000000, -1.000000000000000000 ) ) ;
#8744 = VERTEX_POINT ( 'NONE', #5996 ) ;
#8745 = ORIENTED_EDGE ( 'NONE', *, *, #6617, .T. ) ;
#8746 = CARTESIAN_POINT ( 'NONE',  ( 11.06217782649109260, 10.00000000000000178, -6.386751345948117553 ) ) ;
#8747 = CARTESIAN_POINT ( 'NONE',  ( -10.19839929293505776, 2.531249999044085097, -24.62111388750000174 ) ) ;
#8748 = CARTESIAN_POINT ( 'NONE',  ( -4.522825247065398226E-15, 3.143749999044084475, 24.62111388750000174 ) ) ;
#8749 = ADVANCED_FACE ( 'NONE', ( #5176 ), #975, .F. ) ;
#8750 = CARTESIAN_POINT ( 'NONE',  ( -10.35533905932739174, 3.299999998088169129, 24.99999999999999289 ) ) ;
#8751 = CARTESIAN_POINT ( 'NONE',  ( 25.00000000000000000, 2.000000000000000000, 0.000000000000000000 ) ) ;
#8752 = FACE_OUTER_BOUND ( 'NONE', #645, .T. ) ;
#8753 = CYLINDRICAL_SURFACE ( 'NONE', #7731, 2.999999999999997335 ) ;
#8754 = FACE_OUTER_BOUND ( 'NONE', #7582, .T. ) ;
#8755 = CARTESIAN_POINT ( 'NONE',  ( 17.10400172474269098, -0.001000000000001000089, 9.874999999999957367 ) ) ;
#8756 = FACE_OUTER_BOUND ( 'NONE', #3951, .T. ) ;
#8757 = LINE ( 'NONE', #136, #3205 ) ;
#8758 = ADVANCED_FACE ( 'NONE', ( #5598 ), #6325, .T. ) ;
#8759 = EDGE_LOOP ( 'NONE', ( #3602, #4895, #10123, #8443 ) ) ;
#8760 = ORIENTED_EDGE ( 'NONE', *, *, #778, .F. ) ;
#8761 = CARTESIAN_POINT ( 'NONE',  ( 0.000000000000000000, 8.000000000000000000, 15.00000000000000178 ) ) ;
#8762 = ADVANCED_FACE ( 'NONE', ( #5440, #411 ), #1298, .F. ) ;
#8763 = CARTESIAN_POINT ( 'NONE',  ( 1.530808498934191521E-15, 3.862499998088169573, -25.00000000000000000 ) ) ;
#8764 = DIRECTION ( 'NONE',  ( -0.5000000000000012212, 0.000000000000000000, -0.8660254037844380415 ) ) ;
#8765 = CARTESIAN_POINT ( 'NONE',  ( 1.500000000000001332, 0.000000000000000000, 0.000000000000000000 ) ) ;
#8766 = DIRECTION ( 'NONE',  ( 0.000000000000000000, -1.000000000000000000, 0.000000000000000000 ) ) ;
#8767 = DIRECTION ( 'NONE',  ( 0.000000000000000000, 0.000000000000000000, 1.000000000000000000 ) ) ;
#8768 = EDGE_CURVE ( 'NONE', #10316, #10429, #4774, .T. ) ;
#8769 = CARTESIAN_POINT ( 'NONE',  ( -10.19839929293507552, 4.081249999044084475, 24.62111388749999463 ) ) ;
#8770 = ORIENTED_EDGE ( 'NONE', *, *, #3003, .F. ) ;
#8771 = VERTEX_POINT ( 'NONE', #9014 ) ;
#8772 = ORIENTED_EDGE ( 'NONE', *, *, #8067, .T. ) ;
#8773 = CARTESIAN_POINT ( 'NONE',  ( -17.40975659021753330, 4.018749999044084475, 17.40975659021752975 ) ) ;
#8774 = FACE_OUTER_BOUND ( 'NONE', #9034, .T. ) ;
#8775 = CARTESIAN_POINT ( 'NONE',  ( 6.123233995736763324E-16, 88.00000000000001421, 4.999999999999997335 ) ) ;
#8776 = EDGE_CURVE ( 'NONE', #10147, #2446, #1240, .T. ) ;
#8777 = CARTESIAN_POINT ( 'NONE',  ( 13.63990010960487353, -0.001000000000001000089, -7.875000000000067502 ) ) ;
#8778 = DIRECTION ( 'NONE',  ( 0.000000000000000000, 0.000000000000000000, 1.000000000000000000 ) ) ;
#8779 =( GEOMETRIC_REPRESENTATION_CONTEXT ( 3 ) GLOBAL_UNCERTAINTY_ASSIGNED_CONTEXT ( ( #2278 ) ) GLOBAL_UNIT_ASSIGNED_CONTEXT ( ( #6262, #3866, #445 ) ) REPRESENTATION_CONTEXT ( 'NONE', 'WORKASPACE' ) );
#8780 = VECTOR ( 'NONE', #8863, 999.9999999999998863 ) ;
#8781 = FACE_OUTER_BOUND ( 'NONE', #7485, .T. ) ;
#8782 = CIRCLE ( 'NONE', #2412, 2.999999999999996447 ) ;
#8783 = LINE ( 'NONE', #2198, #5963 ) ;
#8784 = CARTESIAN_POINT ( 'NONE',  ( 3.061616997868383043E-15, 85.00000000000000000, 25.00000000000000000 ) ) ;
#8785 = ORIENTED_EDGE ( 'NONE', *, *, #4313, .F. ) ;
#8786 = CARTESIAN_POINT ( 'NONE',  ( 0.000000000000000000, -1.000000000000003109, -0.5773502691896260641 ) ) ;
#8787 = SHAPE_REPRESENTATION_RELATIONSHIP ( 'NONE' , 'NONE' ,  #7685, #9142 ) ;
#8788 = DIRECTION ( 'NONE',  ( -0.8660254037844399289, 0.000000000000000000, -0.4999999999999977796 ) ) ;
#8789 = VECTOR ( 'NONE', #1704, 1000.000000000000000 ) ;
#8790 = CARTESIAN_POINT ( 'NONE',  ( -17.40975659021752975, 4.593749999044084653, -17.40975659021752975 ) ) ;
#8791 = LINE ( 'NONE', #345, #852 ) ;
#8792 = ORIENTED_EDGE ( 'NONE', *, *, #469, .T. ) ;
#8793 = PRESENTATION_LAYER_ASSIGNMENT (  '', '', ( #9679 ) ) ;
#8794 = APPLICATION_CONTEXT ( 'automotive_design' ) ;
#8795 = VECTOR ( 'NONE', #6357, 1000.000000000000000 ) ;
#8796 = CARTESIAN_POINT ( 'NONE',  ( 10.19839929293505953, 3.406249999044085097, -24.62111388750000174 ) ) ;
#8797 = CARTESIAN_POINT ( 'NONE',  ( -17.40975659021753330, 2.018749999044084475, 17.40975659021752975 ) ) ;
#8798 = CARTESIAN_POINT ( 'NONE',  ( -17.67766952966369232, 2.625000000000000000, 17.67766952966368876 ) ) ;
#8799 =( NAMED_UNIT ( * ) SI_UNIT ( $, .STERADIAN. ) SOLID_ANGLE_UNIT ( ) );
#8800 = LINE ( 'NONE', #7299, #6499 ) ;
#8801 = CARTESIAN_POINT ( 'NONE',  ( 5.237222008264700033E-15, 0.000000000000000000, -0.5000000000000000000 ) ) ;
#8802 = PRODUCT_DEFINITION_CONTEXT ( 'detailed design', #8579, 'design' ) ;
#8803 = DIRECTION ( 'NONE',  ( 0.000000000000000000, -0.000000000000000000, 1.000000000000000000 ) ) ;
#8804 = CARTESIAN_POINT ( 'NONE',  ( -3.223142256880076948E-15, 25.00000000000000000, -15.75000000000000000 ) ) ;
#8805 = ORIENTED_EDGE ( 'NONE', *, *, #10506, .F. ) ;
#8806 = EDGE_CURVE ( 'NONE', #448, #7899, #2111, .T. ) ;
#8807 = EDGE_LOOP ( 'NONE', ( #3889, #8134 ) ) ;
#8808 = FACE_BOUND ( 'NONE', #7649, .T. ) ;
#8809 = DIRECTION ( 'NONE',  ( 0.000000000000000000, 0.000000000000000000, -1.000000000000000000 ) ) ;
#8810 = CARTESIAN_POINT ( 'NONE',  ( -3.957930336368489021E-15, 28.00000000000000000, -19.75000000000000000 ) ) ;
#8811 = CARTESIAN_POINT ( 'NONE',  ( -20.63749999999999929, -1.595945597898662527E-16, -5.750000000000006217 ) ) ;
#8812 = CARTESIAN_POINT ( 'NONE',  ( 0.000000000000000000, 85.00000000000000000, 0.000000000000000000 ) ) ;
#8813 = EDGE_CURVE ( 'NONE', #7572, #5713, #9373, .T. ) ;
#8814 = ORIENTED_EDGE ( 'NONE', *, *, #7971, .F. ) ;
#8815 = EDGE_CURVE ( 'NONE', #10263, #9073, #10621, .T. ) ;
#8816 = CIRCLE ( 'NONE', #4058, 6.999999999999997335 ) ;
#8817 = CIRCLE ( 'NONE', #4948, 2.000000000000000000 ) ;
#8818 = ORIENTED_EDGE ( 'NONE', *, *, #10797, .F. ) ;
#8819 = ADVANCED_FACE ( 'NONE', ( #3088 ), #462, .T. ) ;
#8820 = PRODUCT ( 'BR-816', 'BR-816', '', ( #3982 ) ) ;
#8821 = DIRECTION ( 'NONE',  ( 0.9659258262890684232, -0.2588190451025202399, 0.000000000000000000 ) ) ;
#8822 = CARTESIAN_POINT ( 'NONE',  ( -19.75000000000000000, 28.00000000000000000, 2.108281996628241301E-13 ) ) ;
#8823 = DIRECTION ( 'NONE',  ( 0.000000000000000000, -0.000000000000000000, 1.000000000000000000 ) ) ;
#8824 = VECTOR ( 'NONE', #8433, 1000.000000000000000 ) ;
#8825 = AXIS2_PLACEMENT_3D ( 'NONE', #165, #2633, #5150 ) ;
#8826 = DIRECTION ( 'NONE',  ( -0.000000000000000000, 1.000000000000000000, -0.000000000000000000 ) ) ;
#8827 = CARTESIAN_POINT ( 'NONE',  ( -4.592425496802574367E-15, 1.750000000000000000, 25.00000000000000000 ) ) ;
#8828 = EDGE_CURVE ( 'NONE', #2931, #5067, #8306, .T. ) ;
#8829 = VERTEX_POINT ( 'NONE', #3881 ) ;
#8830 = ORIENTED_EDGE ( 'NONE', *, *, #5831, .F. ) ;
#8831 = AXIS2_PLACEMENT_3D ( 'NONE', #4635, #1254, #6394 ) ;
#8832 = EDGE_CURVE ( 'NONE', #857, #9220, #24, .T. ) ;
#8833 = CARTESIAN_POINT ( 'NONE',  ( 24.62111388750000174, 5.393749999044085364, 0.000000000000000000 ) ) ;
#8834 = DIRECTION ( 'NONE',  ( -1.000000000000000000, 0.000000000000000000, 0.000000000000000000 ) ) ;
#8835 = CARTESIAN_POINT ( 'NONE',  ( -4.592425496802574367E-15, 0.7500000000000000000, 25.00000000000000000 ) ) ;
#8836 = CARTESIAN_POINT ( 'NONE',  ( 6.296693311223896750, 19.03096903053431177, 3.058047309050043960 ) ) ;
#8837 = ORIENTED_EDGE ( 'NONE', *, *, #636, .F. ) ;
#8838 = PLANE ( 'NONE',  #189 ) ;
#8839 = DIRECTION ( 'NONE',  ( 0.000000000000000000, 1.000000000000000000, 0.000000000000000000 ) ) ;
#8840 = ORIENTED_EDGE ( 'NONE', *, *, #10924, .T. ) ;
#8841 = CARTESIAN_POINT ( 'NONE',  ( 10.19839929293506486, 3.031249999044084653, 24.62111388749999819 ) ) ;
#8842 = CARTESIAN_POINT ( 'NONE',  ( 0.000000000000000000, 20.00000000000000355, -6.999999999999997335 ) ) ;
#8843 = AXIS2_PLACEMENT_3D ( 'NONE', #10795, #7414, #3201 ) ;
#8844 = EDGE_LOOP ( 'NONE', ( #10005, #464, #2492, #3165 ) ) ;
#8845 = AXIS2_PLACEMENT_3D ( 'NONE', #6546, #3311, #7644 ) ;
#8846 = CARTESIAN_POINT ( 'NONE',  ( 27.32050807568876749, 100.0000000000000142, -5.000000000000000000 ) ) ;
#8847 = CARTESIAN_POINT ( 'NONE',  ( -24.62111388750000174, 4.718749999044084653, -3.015216831376932151E-15 ) ) ;
#8848 = CARTESIAN_POINT ( 'NONE',  ( 1.507608415688466075E-15, 3.643749999044084920, -24.62111388750000174 ) ) ;
#8849 = VERTEX_POINT ( 'NONE', #3831 ) ;
#8850 = DIRECTION ( 'NONE',  ( 0.000000000000000000, 0.000000000000000000, 1.000000000000000000 ) ) ;
#8851 = SURFACE_SIDE_STYLE ('',( #8522 ) ) ;
#8852 = VECTOR ( 'NONE', #4648, 1000.000000000000000 ) ;
#8853 = DIRECTION ( 'NONE',  ( 1.000000000000000000, 0.000000000000000000, 0.000000000000000000 ) ) ;
#8854 = CARTESIAN_POINT ( 'NONE',  ( 10.35533905932737930, 0.7999999980881692396, -25.00000000000000000 ) ) ;
#8855 = CARTESIAN_POINT ( 'NONE',  ( 3.418204983771597728E-15, -8.000000000000000000, 27.91176187412962761 ) ) ;
#8856 = DIRECTION ( 'NONE',  ( 1.000000000000000000, 0.000000000000000000, 0.000000000000000000 ) ) ;
#8857 = CARTESIAN_POINT ( 'NONE',  ( -25.00000000000000000, 2.500000000000000000, -3.061616997868383043E-15 ) ) ;
#8858 = AXIS2_PLACEMENT_3D ( 'NONE', #2190, #5568, #7316 ) ;
#8859 = ORIENTED_EDGE ( 'NONE', *, *, #4218, .F. ) ;
#8860 = ORIENTED_EDGE ( 'NONE', *, *, #196, .F. ) ;
#8861 = ORIENTED_EDGE ( 'NONE', *, *, #3060, .T. ) ;
#8862 = VERTEX_POINT ( 'NONE', #10519 ) ;
#8863 = DIRECTION ( 'NONE',  ( 0.000000000000000000, -0.9396926207859082059, -0.3420201433256694901 ) ) ;
#8864 = AXIS2_PLACEMENT_3D ( 'NONE', #8590, #3506, #7654 ) ;
#8865 = DIRECTION ( 'NONE',  ( 1.445602896647339163E-16, 0.000000000000000000, 1.000000000000000000 ) ) ;
#8866 = DIRECTION ( 'NONE',  ( 0.000000000000000000, -9.470910429910653047E-17, 1.000000000000000000 ) ) ;
#8867 = AXIS2_PLACEMENT_3D ( 'NONE', #8716, #4537, #8654 ) ;
#8868 = LINE ( 'NONE', #1308, #728 ) ;
#8869 = AXIS2_PLACEMENT_3D ( 'NONE', #8364, #7532, #9963 ) ;
#8870 = DIRECTION ( 'NONE',  ( 0.000000000000000000, 1.000000000000000000, 0.000000000000000000 ) ) ;
#8871 = LINE ( 'NONE', #8092, #6047 ) ;
#8872 = VERTEX_POINT ( 'NONE', #3036 ) ;
#8873 = AXIS2_PLACEMENT_3D ( 'NONE', #2865, #4442, #3813 ) ;
#8874 = ORIENTED_EDGE ( 'NONE', *, *, #3199, .T. ) ;
#8875 = CIRCLE ( 'NONE', #587, 5.349378127920655146 ) ;
#8876 = DIRECTION ( 'NONE',  ( 0.000000000000000000, -1.000000000000000000, 0.000000000000000000 ) ) ;
#8877 = EDGE_CURVE ( 'NONE', #9337, #3918, #217, .T. ) ;
#8878 = AXIS2_PLACEMENT_3D ( 'NONE', #7775, #5299, #10365 ) ;
#8879 = CARTESIAN_POINT ( 'NONE',  ( 0.000000000000000000, 85.00000000000000000, 0.000000000000000000 ) ) ;
#8880 = VECTOR ( 'NONE', #434, 1000.000000000000000 ) ;
#8881 = DIRECTION ( 'NONE',  ( 0.000000000000000000, 0.000000000000000000, 1.000000000000000000 ) ) ;
#8882 = DIRECTION ( 'NONE',  ( 0.000000000000000000, 0.000000000000000000, 1.000000000000000000 ) ) ;
#8883 = LINE ( 'NONE', #1317, #1999 ) ;
#8884 = AXIS2_PLACEMENT_3D ( 'NONE', #161, #5372, #8823 ) ;
#8885 = EDGE_CURVE ( 'NONE', #10673, #3501, #9786, .T. ) ;
#8886 = ORIENTED_EDGE ( 'NONE', *, *, #4926, .F. ) ;
#8887 = CIRCLE ( 'NONE', #7472, 5.000000000000000888 ) ;
#8888 = EDGE_LOOP ( 'NONE', ( #4269, #8687, #4795, #10805 ) ) ;
#8889 = CYLINDRICAL_SURFACE ( 'NONE', #3330, 5.000000000000000888 ) ;
#8890 = PLANE ( 'NONE',  #8066 ) ;
#8891 = LINE ( 'NONE', #6417, #9737 ) ;
#8892 = ORIENTED_EDGE ( 'NONE', *, *, #4549, .F. ) ;
#8893 = EDGE_CURVE ( 'NONE', #8398, #6763, #1439, .T. ) ;
#8894 = DIRECTION ( 'NONE',  ( 1.000000000000000000, 0.000000000000000000, 0.000000000000000000 ) ) ;
#8895 = DIRECTION ( 'NONE',  ( 0.000000000000000000, 1.000000000000000000, 0.000000000000000000 ) ) ;
#8896 = CARTESIAN_POINT ( 'NONE',  ( 24.62111388750000174, 3.218749999044084653, 0.000000000000000000 ) ) ;
#8897 = CARTESIAN_POINT ( 'NONE',  ( -0.5000000000000000000, 10.00000000000000355, -6.982120021884467675 ) ) ;
#8898 = EDGE_CURVE ( 'NONE', #6538, #2980, #5168, .T. ) ;
#8899 = ORIENTED_EDGE ( 'NONE', *, *, #865, .F. ) ;
#8900 = ORIENTED_EDGE ( 'NONE', *, *, #8601, .T. ) ;
#8901 = ORIENTED_EDGE ( 'NONE', *, *, #4051, .F. ) ;
#8902 = LINE ( 'NONE', #8846, #5662 ) ;
#8903 = CARTESIAN_POINT ( 'NONE',  ( -10.19839929293505776, 4.531249999044084653, -24.62111388750000174 ) ) ;
#8904 = CARTESIAN_POINT ( 'NONE',  ( 10.19839929293506486, 3.206249999044084031, 24.62111388749999819 ) ) ;
#8905 = CARTESIAN_POINT ( 'NONE',  ( 24.99999999999999289, 3.937500000000000000, 10.35533905932739529 ) ) ;
#8906 =( NAMED_UNIT ( * ) SI_UNIT ( $, .STERADIAN. ) SOLID_ANGLE_UNIT ( ) );
#8907 = DIRECTION ( 'NONE',  ( 1.000000000000000000, 0.000000000000000000, 0.000000000000000000 ) ) ;
#8908 = CARTESIAN_POINT ( 'NONE',  ( -10.35533905932737575, 1.924999998088169129, -25.00000000000000000 ) ) ;
#8909 = DIRECTION ( 'NONE',  ( 1.000000000000000000, 0.000000000000000000, 0.000000000000000000 ) ) ;
#8910 = DIRECTION ( 'NONE',  ( 0.8660254037844363761, 0.000000000000000000, 0.5000000000000039968 ) ) ;
#8911 = ADVANCED_FACE ( 'NONE', ( #7201 ), #2928, .F. ) ;
#8912 = ORIENTED_EDGE ( 'NONE', *, *, #9892, .F. ) ;
#8913 = ORIENTED_EDGE ( 'NONE', *, *, #7810, .T. ) ;
#8914 = DIRECTION ( 'NONE',  ( 0.000000000000000000, -0.8660254037844391517, -0.4999999999999992784 ) ) ;
#8915 = CARTESIAN_POINT ( 'NONE',  ( 3.785909150703014259, 19.34316356887877575, 5.890223162633890119 ) ) ;
#8916 = CARTESIAN_POINT ( 'NONE',  ( 17.10400172474269098, -0.001000000000001000089, 9.874999999999957367 ) ) ;
#8917 = DIRECTION ( 'NONE',  ( 0.8660254037844402619, -0.4999999999999970579, 0.000000000000000000 ) ) ;
#8918 = DIRECTION ( 'NONE',  ( -0.000000000000000000, 1.000000000000000000, -0.000000000000000000 ) ) ;
#8919 = CARTESIAN_POINT ( 'NONE',  ( 2.449293598294706513E-15, 20.00000000000000355, -20.00000000000000000 ) ) ;
#8920 = FACE_OUTER_BOUND ( 'NONE', #8215, .T. ) ;
#8921 = EDGE_LOOP ( 'NONE', ( #5629, #3917 ) ) ;
#8922 = ORIENTED_EDGE ( 'NONE', *, *, #1157, .T. ) ;
#8923 = ORIENTED_EDGE ( 'NONE', *, *, #5600, .T. ) ;
#8924 = VERTEX_POINT ( 'NONE', #8855 ) ;
#8925 = CARTESIAN_POINT ( 'NONE',  ( -19.05903902044739695, 4.999999999999999112, -16.17878337876688022 ) ) ;
#8926 = CARTESIAN_POINT ( 'NONE',  ( 25.00000000000000000, 0.6124999980881691286, 0.000000000000000000 ) ) ;
#8927 = DIRECTION ( 'NONE',  ( 0.5000000000000009992, 0.8660254037844380415, 5.237222008264710288E-15 ) ) ;
#8928 = CARTESIAN_POINT ( 'NONE',  ( 3.061616997868383043E-15, 5.000000000000000000, 25.00000000000000000 ) ) ;
#8929 = CARTESIAN_POINT ( 'NONE',  ( -1.399999999999998579, -2.081668171172168513E-16, -7.500000000000007994 ) ) ;
#8930 = APPLICATION_CONTEXT ( 'automotive_design' ) ;
#8931 = ADVANCED_FACE ( 'NONE', ( #2976 ), #6384, .F. ) ;
#8932 = ORIENTED_EDGE ( 'NONE', *, *, #8685, .T. ) ;
#8933 =( BOUNDED_CURVE ( )  B_SPLINE_CURVE ( 2, ( #4307, #98, #9097, #1528, #3224, #8260, #704, #4083, #10824, #6621, #8667, #9379, #1051, #1821, #7902, #10380, #9443, #1169, #1876, #7851, #2685, #5255, #6190, #10433, #2740, #2793, #3637, #5207, #9555, #6085, #10328, #7021, #6249, #3518, #6973, #1992, #8548, #1214, #10488, #5368, #7124, #5310, #8727, #325, #9609, #4546, #6133, #2041, #4595, #3692, #275, #7074, #3580, #2848, #1110, #9498, #8604, #5415, #8773, #995, #4491, #7945, #376, #3745, #6022, #1932, #218, #4360, #7725, #4423, #7788, #158, #6914, #10267, #480 ),
 .UNSPECIFIED., .F., .F. ) 
 B_SPLINE_CURVE_WITH_KNOTS ( ( 3, 2, 2, 2, 2, 2, 2, 2, 2, 2, 2, 2, 2, 2, 2, 2, 2, 2, 2, 2, 2, 2, 2, 2, 2, 2, 2, 2, 2, 2, 2, 2, 2, 2, 2, 2, 2, 3 ),
 ( 0.000000000000000000, 0.02500000000000000139, 0.05000000000000000278, 0.07499999999999999722, 0.1000000000000000056, 0.1250000000000000000, 0.1499999999999999944, 0.1749999999999999889, 0.2000000000000000111, 0.2250000000000000056, 0.2500000000000000000, 0.2750000000000000222, 0.2999999999999999889, 0.3250000000000000111, 0.3499999999999999778, 0.3750000000000000000, 0.4000000000000000222, 0.4249999999999999889, 0.4500000000000000111, 0.4749999999999999778, 0.5000000000000000000, 0.5250000000000000222, 0.5500000000000000444, 0.5749999999999999556, 0.5999999999999999778, 0.6250000000000000000, 0.6500000000000000222, 0.6750000000000000444, 0.6999999999999999556, 0.7249999999999999778, 0.7500000000000000000, 0.7750000000000000222, 0.8000000000000000444, 0.8249999999999999556, 0.8499999999999999778, 0.8750000000000000000, 0.9000000000000000222, 0.9210736448048598701 ),
 .UNSPECIFIED. ) 
 CURVE ( )  GEOMETRIC_REPRESENTATION_ITEM ( )  RATIONAL_B_SPLINE_CURVE ( ( 1.000000000000000000, 0.9238795325112867385, 1.000000000000000000, 0.9238795325112867385, 1.000000000000000000, 0.9238795325112867385, 1.000000000000000000, 0.9238795325112867385, 1.000000000000000000, 0.9238795325112867385, 1.000000000000000000, 0.9238795325112867385, 1.000000000000000000, 0.9238795325112867385, 1.000000000000000000, 0.9238795325112867385, 1.000000000000000000, 0.9238795325112867385, 1.000000000000000000, 0.9238795325112867385, 1.000000000000000000, 0.9238795325112867385, 1.000000000000000000, 0.9238795325112867385, 1.000000000000000000, 0.9238795325112867385, 1.000000000000000000, 0.9238795325112867385, 1.000000000000000000, 0.9238795325112867385, 1.000000000000000000, 0.9238795325112867385, 1.000000000000000000, 0.9238795325112867385, 1.000000000000000000, 0.9238795325112867385, 1.000000000000000000, 0.9238795325112867385, 1.000000000000000000, 0.9238795325112867385, 1.000000000000000000, 0.9238795325112867385, 1.000000000000000000, 0.9238795325112867385, 1.000000000000000000, 0.9238795325112867385, 1.000000000000000000, 0.9238795325112867385, 1.000000000000000000, 0.9238795325112867385, 1.000000000000000000, 0.9238795325112867385, 1.000000000000000000, 0.9238795325112867385, 1.000000000000000000, 0.9238795325112867385, 1.000000000000000000, 0.9238795325112867385, 1.000000000000000000, 0.9238795325112867385, 1.000000000000000000, 0.9238795325112867385, 1.000000000000000000, 0.9238795325112867385, 1.000000000000000000, 0.9238795325112867385, 1.000000000000000000, 0.9238795325112867385, 1.000000000000000000, 0.9238795325112867385, 1.000000000000000000, 0.9238795325112867385, 1.000000000000000000, 0.9358345722305186909, 0.9798450991463130144 ) ) 
 REPRESENTATION_ITEM ( '' )  );
#8934 = LINE ( 'NONE', #10757, #8293 ) ;
#8935 = CARTESIAN_POINT ( 'NONE',  ( -9.874999999999777955, 28.00000000000000000, 17.10400172474279401 ) ) ;
#8936 = CARTESIAN_POINT ( 'NONE',  ( -10.19839929293505776, 3.706249999044085808, -24.62111388750000174 ) ) ;
#8937 = ORIENTED_EDGE ( 'NONE', *, *, #10774, .T. ) ;
#8938 = LINE ( 'NONE', #4756, #8987 ) ;
#8939 = EDGE_CURVE ( 'NONE', #6845, #8744, #10618, .T. ) ;
#8940 = CARTESIAN_POINT ( 'NONE',  ( 0.000000000000000000, 25.00000000000000000, 0.000000000000000000 ) ) ;
#8941 = VERTEX_POINT ( 'NONE', #8348 ) ;
#8942 = STYLED_ITEM ( 'NONE', ( #494 ), #4414 ) ;
#8943 = CARTESIAN_POINT ( 'NONE',  ( 10.19839929293505953, 3.406249999044085097, -24.62111388750000174 ) ) ;
#8944 = CARTESIAN_POINT ( 'NONE',  ( 10.35533905932738286, 2.424999998088169129, 24.99999999999999645 ) ) ;
#8945 = EDGE_LOOP ( 'NONE', ( #3133, #5580, #7364, #10393, #9809 ) ) ;
#8946 = ORIENTED_EDGE ( 'NONE', *, *, #4396, .F. ) ;
#8947 = EDGE_CURVE ( 'NONE', #917, #8872, #6231, .T. ) ;
#8948 = ORIENTED_EDGE ( 'NONE', *, *, #6061, .F. ) ;
#8949 = EDGE_CURVE ( 'NONE', #1513, #6058, #1436, .T. ) ;
#8950 = CIRCLE ( 'NONE', #1209, 2.999999999999997335 ) ;
#8951 = CARTESIAN_POINT ( 'NONE',  ( -4.522825247065398226E-15, 1.143749999044084475, 24.62111388750000174 ) ) ;
#8952 = CARTESIAN_POINT ( 'NONE',  ( 15.74999999999999289, 25.00000000000000000, -3.000000000000053291 ) ) ;
#8953 = CARTESIAN_POINT ( 'NONE',  ( 24.62111388749999463, 3.331249999044084920, 10.19839929293507730 ) ) ;
#8954 = ORIENTED_EDGE ( 'NONE', *, *, #3392, .F. ) ;
#8955 = CARTESIAN_POINT ( 'NONE',  ( -25.00000000000000000, 4.437500000000000888, -10.35533905932738108 ) ) ;
#8956 = SURFACE_STYLE_USAGE ( .BOTH. , #8851 ) ;
#8957 = EDGE_CURVE ( 'NONE', #3717, #1851, #5048, .T. ) ;
#8958 = DIRECTION ( 'NONE',  ( 0.000000000000000000, 1.000000000000000000, 0.000000000000000000 ) ) ;
#8959 = CARTESIAN_POINT ( 'NONE',  ( -2.999999999999996447, 28.00000000000000000, 19.75000000000000000 ) ) ;
#8960 = CARTESIAN_POINT ( 'NONE',  ( 25.00000000000000000, 1.062500000000000222, -10.35533905932737753 ) ) ;
#8961 = TOROIDAL_SURFACE ( 'NONE', #3848, 3.379762621896238883, 2.000000000000000000 ) ;
#8962 = CIRCLE ( 'NONE', #10194, 5.000000000000000000 ) ;
#8963 = ORIENTED_EDGE ( 'NONE', *, *, #8813, .F. ) ;
#8964 = ADVANCED_FACE ( 'NONE', ( #6641 ), #2533, .T. ) ;
#8965 = ORIENTED_EDGE ( 'NONE', *, *, #5914, .F. ) ;
#8966 = ORIENTED_EDGE ( 'NONE', *, *, #7804, .T. ) ;
#8967 = DIRECTION ( 'NONE',  ( 1.000000000000000000, 0.000000000000000000, 0.000000000000000000 ) ) ;
#8968 = DIRECTION ( 'NONE',  ( 0.000000000000000000, -1.000000000000000000, 0.000000000000000000 ) ) ;
#8969 = CARTESIAN_POINT ( 'NONE',  ( 2.500000000000000444, -1.000000000000003331, 0.5773502691896272854 ) ) ;
#8970 = EDGE_CURVE ( 'NONE', #2933, #5713, #7402, .T. ) ;
#8971 = AXIS2_PLACEMENT_3D ( 'NONE', #1579, #763, #7497 ) ;
#8972 = DIRECTION ( 'NONE',  ( 0.000000000000000000, 0.000000000000000000, 1.000000000000000000 ) ) ;
#8973 = CARTESIAN_POINT ( 'NONE',  ( -11.06217782649114589, 10.00000000000000355, 6.386751345948025183 ) ) ;
#8974 = LINE ( 'NONE', #1309, #4621 ) ;
#8975 = DIRECTION ( 'NONE',  ( 0.000000000000000000, 0.000000000000000000, 1.000000000000000000 ) ) ;
#8976 = ORIENTED_EDGE ( 'NONE', *, *, #8970, .F. ) ;
#8977 = ORIENTED_EDGE ( 'NONE', *, *, #1576, .T. ) ;
#8978 = ORIENTED_EDGE ( 'NONE', *, *, #3573, .T. ) ;
#8979 = VERTEX_POINT ( 'NONE', #838 ) ;
#8980 = EDGE_CURVE ( 'NONE', #6448, #10381, #8229, .T. ) ;
#8981 = DIRECTION ( 'NONE',  ( 1.000000000000000000, 0.000000000000000000, 0.000000000000000000 ) ) ;
#8982 = DIRECTION ( 'NONE',  ( 1.000000000000000000, 0.000000000000000000, 0.000000000000000000 ) ) ;
#8983 = PLANE ( 'NONE',  #10121 ) ;
#8984 = CARTESIAN_POINT ( 'NONE',  ( -13.63990010960498367, 25.00000000000000000, -4.874999999999871214 ) ) ;
#8985 = DIRECTION ( 'NONE',  ( 0.8660254037844397068, 0.000000000000000000, -0.4999999999999979461 ) ) ;
#8986 = AXIS2_PLACEMENT_3D ( 'NONE', #558, #1387, #4773 ) ;
#8987 = VECTOR ( 'NONE', #8212, 1000.000000000000000 ) ;
#8988 = LINE ( 'NONE', #7225, #9715 ) ;
#8989 = PRESENTATION_STYLE_ASSIGNMENT (( #650 ) ) ;
#8990 = AXIS2_PLACEMENT_3D ( 'NONE', #7343, #719, #3991 ) ;
#8991 = CARTESIAN_POINT ( 'NONE',  ( -4.522825247065398226E-15, 3.143749999044084475, 24.62111388750000174 ) ) ;
#8992 = ORIENTED_EDGE ( 'NONE', *, *, #5978, .T. ) ;
#8993 = CARTESIAN_POINT ( 'NONE',  ( 1.530808498934191521E-15, 3.862499998088169573, -25.00000000000000000 ) ) ;
#8994 =( NAMED_UNIT ( * ) SI_UNIT ( $, .STERADIAN. ) SOLID_ANGLE_UNIT ( ) );
#8995 = CARTESIAN_POINT ( 'NONE',  ( 10.35533905932738286, 2.424999998088169129, 24.99999999999999645 ) ) ;
#8996 = ORIENTED_EDGE ( 'NONE', *, *, #9759, .T. ) ;
#8997 = CARTESIAN_POINT ( 'NONE',  ( 0.000000000000000000, 10.00000000000000355, 0.000000000000000000 ) ) ;
#8998 = CARTESIAN_POINT ( 'NONE',  ( 24.62111388749999108, 3.156249999044084653, 10.19839929293507730 ) ) ;
#8999 = EDGE_LOOP ( 'NONE', ( #5928, #9943, #2590, #4487, #3887 ) ) ;
#9000 = VECTOR ( 'NONE', #10581, 1000.000000000000000 ) ;
#9001 = ORIENTED_EDGE ( 'NONE', *, *, #9661, .F. ) ;
#9002 = VECTOR ( 'NONE', #8914, 999.9999999999998863 ) ;
#9003 =( BOUNDED_CURVE ( )  B_SPLINE_CURVE ( 3, ( #8608, #1767, #9318, #3523 ),
 .UNSPECIFIED., .F., .F. ) 
 B_SPLINE_CURVE_WITH_KNOTS ( ( 4, 4 ),
 ( 2.284520705739661484, 2.356010155625182012 ),
 .UNSPECIFIED. ) 
 CURVE ( )  GEOMETRIC_REPRESENTATION_ITEM ( )  RATIONAL_B_SPLINE_CURVE ( ( 1.000000000000000000, 0.9995741502243209453, 0.9995741502243209453, 1.000000000000000000 ) ) 
 REPRESENTATION_ITEM ( '' )  );
#9004 = CARTESIAN_POINT ( 'NONE',  ( 17.67766952966369232, 4.737499998088169129, -17.67766952966369232 ) ) ;
#9005 = FACE_OUTER_BOUND ( 'NONE', #5628, .T. ) ;
#9006 = CARTESIAN_POINT ( 'NONE',  ( -24.62111388750000174, 2.718749999044084653, -3.015216831376932151E-15 ) ) ;
#9007 = CARTESIAN_POINT ( 'NONE',  ( 7.874999999999916511, 25.00000000000000000, -10.63990010960495702 ) ) ;
#9008 = AXIS2_PLACEMENT_3D ( 'NONE', #5654, #10726, #5710 ) ;
#9009 = CIRCLE ( 'NONE', #8273, 2.999999999999999112 ) ;
#9010 = EDGE_CURVE ( 'NONE', #8258, #2606, #2428, .T. ) ;
#9011 = CARTESIAN_POINT ( 'NONE',  ( -5.796693311223863887, 10.00000000000000355, -3.924072712834521415 ) ) ;
#9012 = CARTESIAN_POINT ( 'NONE',  ( -10.35533905932739174, 1.299999998088169129, 24.99999999999999289 ) ) ;
#9013 = EDGE_CURVE ( 'NONE', #564, #10147, #4992, .T. ) ;
#9014 = CARTESIAN_POINT ( 'NONE',  ( 10.31217782649105352, 10.00000000000000355, 6.531088913245589822 ) ) ;
#9015 = DIRECTION ( 'NONE',  ( 0.000000000000000000, -2.775557561562888270E-17, -1.000000000000000000 ) ) ;
#9016 = ORIENTED_EDGE ( 'NONE', *, *, #994, .T. ) ;
#9017 = ORIENTED_EDGE ( 'NONE', *, *, #3282, .T. ) ;
#9018 = ORIENTED_EDGE ( 'NONE', *, *, #2585, .T. ) ;
#9019 = EDGE_CURVE ( 'NONE', #5067, #3964, #788, .T. ) ;
#9020 = EDGE_LOOP ( 'NONE', ( #2300, #3166, #9724, #4918 ) ) ;
#9021 = UNCERTAINTY_MEASURE_WITH_UNIT (LENGTH_MEASURE( 1.000000000000000082E-05 ), #10704, 'distance_accuracy_value', 'NONE');
#9022 = CARTESIAN_POINT ( 'NONE',  ( 0.000000000000000000, 8.000000000000003553, 0.000000000000000000 ) ) ;
#9023 = CARTESIAN_POINT ( 'NONE',  ( 24.62111388750000174, 0.2187499990440845699, 0.000000000000000000 ) ) ;
#9024 = ORIENTED_EDGE ( 'NONE', *, *, #1723, .F. ) ;
#9025 = EDGE_CURVE ( 'NONE', #257, #8103, #4637, .T. ) ;
#9026 = LINE ( 'NONE', #8145, #6970 ) ;
#9027 = LINE ( 'NONE', #4848, #3359 ) ;
#9028 = CARTESIAN_POINT ( 'NONE',  ( 17.40975659021752620, 4.093749999044084653, 17.40975659021753330 ) ) ;
#9029 = CARTESIAN_POINT ( 'NONE',  ( -17.67766952966368876, 3.375000000000000000, -17.67766952966369232 ) ) ;
#9030 = ORIENTED_EDGE ( 'NONE', *, *, #5774, .T. ) ;
#9031 = EDGE_CURVE ( 'NONE', #7140, #10484, #7518, .T. ) ;
#9032 = VECTOR ( 'NONE', #9948, 1000.000000000000000 ) ;
#9033 = ORIENTED_EDGE ( 'NONE', *, *, #2984, .T. ) ;
#9034 = EDGE_LOOP ( 'NONE', ( #306, #9111, #9187, #181 ) ) ;
#9035 = ADVANCED_FACE ( 'NONE', ( #3357, #6757 ), #5810, .T. ) ;
#9036 = ORIENTED_EDGE ( 'NONE', *, *, #7404, .T. ) ;
#9037 = CIRCLE ( 'NONE', #739, 22.00000000000000355 ) ;
#9038 = VERTEX_POINT ( 'NONE', #5868 ) ;
#9039 = VECTOR ( 'NONE', #8197, 1000.000000000000000 ) ;
#9040 = CYLINDRICAL_SURFACE ( 'NONE', #3380, 25.00000000000000000 ) ;
#9041 = CYLINDRICAL_SURFACE ( 'NONE', #2022, 24.91176187412963117 ) ;
#9042 = CARTESIAN_POINT ( 'NONE',  ( -2.999999999999996447, 28.00000000000000000, 19.75000000000000000 ) ) ;
#9043 = CARTESIAN_POINT ( 'NONE',  ( 0.000000000000000000, 10.00000000000000355, 0.000000000000000000 ) ) ;
#9044 = CARTESIAN_POINT ( 'NONE',  ( 24.81055694375000087, 0.1093749995220422710, 0.000000000000000000 ) ) ;
#9045 = AXIS2_PLACEMENT_3D ( 'NONE', #5072, #21, #7541 ) ;
#9046 = AXIS2_PLACEMENT_3D ( 'NONE', #7308, #10688, #4062 ) ;
#9047 = ADVANCED_FACE ( 'NONE', ( #3241 ), #9273, .T. ) ;
#9048 = CIRCLE ( 'NONE', #7274, 2.999999999999997780 ) ;
#9049 = ORIENTED_EDGE ( 'NONE', *, *, #4926, .T. ) ;
#9050 = AXIS2_PLACEMENT_3D ( 'NONE', #9691, #8088, #3238 ) ;
#9051 = AXIS2_PLACEMENT_3D ( 'NONE', #5025, #1749, #4350 ) ;
#9052 =( NAMED_UNIT ( * ) SI_UNIT ( $, .STERADIAN. ) SOLID_ANGLE_UNIT ( ) );
#9053 = CARTESIAN_POINT ( 'NONE',  ( 1.507608415688466075E-15, 4.643749999044084475, -24.62111388750000174 ) ) ;
#9054 = ORIENTED_EDGE ( 'NONE', *, *, #8555, .F. ) ;
#9055 = DIRECTION ( 'NONE',  ( 0.8660254037844363761, 0.000000000000000000, 0.5000000000000039968 ) ) ;
#9056 = DIRECTION ( 'NONE',  ( 0.2157500049970334233, 0.000000000000000000, 0.9764486342577269884 ) ) ;
#9057 = DIRECTION ( 'NONE',  ( 0.000000000000000000, -1.000000000000000000, 0.000000000000000000 ) ) ;
#9058 = PLANE ( 'NONE',  #7996 ) ;
#9059 = CARTESIAN_POINT ( 'NONE',  ( 24.62111388750000174, 0.2812499990440845421, -10.19839929293505776 ) ) ;
#9060 = ORIENTED_EDGE ( 'NONE', *, *, #8257, .F. ) ;
#9061 = CONICAL_SURFACE ( 'NONE', #6590, 20.00000000000000000, 0.3947911196997613281 ) ;
#9062 = ORIENTED_EDGE ( 'NONE', *, *, #119, .T. ) ;
#9063 = CIRCLE ( 'NONE', #6968, 4.500000000000000888 ) ;
#9064 = CARTESIAN_POINT ( 'NONE',  ( 25.00000000000000000, 3.612499998088169129, 0.000000000000000000 ) ) ;
#9065 = CARTESIAN_POINT ( 'NONE',  ( 11.06217782649104997, 10.00000000000000355, 6.386751345948187719 ) ) ;
#9066 = CARTESIAN_POINT ( 'NONE',  ( -4.522825247065398226E-15, 5.143749999044084475, 24.62111388750000174 ) ) ;
#9067 = LINE ( 'NONE', #666, #9862 ) ;
#9068 = CYLINDRICAL_SURFACE ( 'NONE', #1212, 2.999999999999997335 ) ;
#9069 = DIRECTION ( 'NONE',  ( -0.000000000000000000, 1.000000000000000000, 0.000000000000000000 ) ) ;
#9070 = DIRECTION ( 'NONE',  ( 1.000000000000000000, 0.000000000000000000, 0.000000000000000000 ) ) ;
#9071 = CARTESIAN_POINT ( 'NONE',  ( 3.061616997868383043E-15, 85.00000000000000000, 25.00000000000000000 ) ) ;
#9072 = ORIENTED_EDGE ( 'NONE', *, *, #7389, .F. ) ;
#9073 = VERTEX_POINT ( 'NONE', #4158 ) ;
#9074 = ORIENTED_EDGE ( 'NONE', *, *, #9976, .F. ) ;
#9075 = EDGE_CURVE ( 'NONE', #2200, #652, #1501, .T. ) ;
#9076 = CARTESIAN_POINT ( 'NONE',  ( 17.67766952966369232, 3.125000000000000000, -17.67766952966369232 ) ) ;
#9077 = DIRECTION ( 'NONE',  ( 0.000000000000000000, 1.000000000000000000, 0.000000000000000000 ) ) ;
#9078 = LINE ( 'NONE', #5610, #5546 ) ;
#9079 = ADVANCED_FACE ( 'NONE', ( #725 ), #10725, .T. ) ;
#9080 = CARTESIAN_POINT ( 'NONE',  ( -17.10400172474254532, 25.00000000000000000, 9.875000000000202505 ) ) ;
#9081 = CARTESIAN_POINT ( 'NONE',  ( 24.62111388749999463, 3.156249999044084653, 10.19839929293507730 ) ) ;
#9082 = CARTESIAN_POINT ( 'NONE',  ( 0.5000000000000000000, 19.74999999999999645, -6.566987298107768822 ) ) ;
#9083 = ORIENTED_EDGE ( 'NONE', *, *, #10855, .F. ) ;
#9084 = VERTEX_POINT ( 'NONE', #4106 ) ;
#9085 = EDGE_CURVE ( 'NONE', #3717, #417, #1109, .T. ) ;
#9086 = ORIENTED_EDGE ( 'NONE', *, *, #10904, .T. ) ;
#9087 = DIRECTION ( 'NONE',  ( -0.1767766952966274840, 0.3535533905932751741, -0.9185586535436930378 ) ) ;
#9088 = CYLINDRICAL_SURFACE ( 'NONE', #5203, 25.00000000000000000 ) ;
#9089 = EDGE_CURVE ( 'NONE', #7005, #9938, #6040, .T. ) ;
#9090 = CARTESIAN_POINT ( 'NONE',  ( 7.874999999999916511, 28.00000000000000000, -13.63990010960495702 ) ) ;
#9091 = CARTESIAN_POINT ( 'NONE',  ( 10.35533905932739174, 0.8125000000000001110, 24.99999999999998934 ) ) ;
#9092 = PLANE ( 'NONE',  #7813 ) ;
#9093 = ORIENTED_EDGE ( 'NONE', *, *, #7742, .T. ) ;
#9094 = EDGE_LOOP ( 'NONE', ( #10124, #9438, #4330, #9968 ) ) ;
#9095 = DIRECTION ( 'NONE',  ( 0.000000000000000000, 1.000000000000000000, 0.000000000000000000 ) ) ;
#9096 = CARTESIAN_POINT ( 'NONE',  ( -5.999999999999992895, 10.00000000000000355, -0.5000000000000628386 ) ) ;
#9097 = CARTESIAN_POINT ( 'NONE',  ( 17.40975659021752975, 0.5187499990440845865, -17.40975659021752975 ) ) ;
#9098 = EDGE_CURVE ( 'NONE', #10429, #5999, #5158, .T. ) ;
#9099 = ORIENTED_EDGE ( 'NONE', *, *, #6211, .T. ) ;
#9100 = CARTESIAN_POINT ( 'NONE',  ( 7.856406460551036197, 98.00000000000001421, 5.000000000000000000 ) ) ;
#9101 = CARTESIAN_POINT ( 'NONE',  ( 17.67766952966368521, 2.487499998088169129, 17.67766952966369232 ) ) ;
#9102 = PLANE ( 'NONE',  #10469 ) ;
#9103 = CARTESIAN_POINT ( 'NONE',  ( 1.507608415688466075E-15, 2.468749999044085097, -24.62111388750000174 ) ) ;
#9104 = ORIENTED_EDGE ( 'NONE', *, *, #1525, .F. ) ;
#9105 = VERTEX_POINT ( 'NONE', #3477 ) ;
#9106 = ORIENTED_EDGE ( 'NONE', *, *, #5552, .T. ) ;
#9107 = EDGE_CURVE ( 'NONE', #2032, #963, #10492, .T. ) ;
#9108 = CARTESIAN_POINT ( 'NONE',  ( 10.19839929293506486, 5.031249999044083765, 24.62111388749999819 ) ) ;
#9109 = PRESENTATION_LAYER_ASSIGNMENT (  '', '', ( #10889 ) ) ;
#9110 = CARTESIAN_POINT ( 'NONE',  ( -24.62111388750000884, 2.781249999044085541, 10.19839929293505421 ) ) ;
#9111 = ORIENTED_EDGE ( 'NONE', *, *, #5799, .T. ) ;
#9112 = CARTESIAN_POINT ( 'NONE',  ( 0.000000000000000000, 20.00000000000000355, -6.999999999999997335 ) ) ;
#9113 =( LENGTH_UNIT ( ) NAMED_UNIT ( * ) SI_UNIT ( .MILLI., .METRE. ) );
#9114 = LINE ( 'NONE', #2268, #3122 ) ;
#9115 = LINE ( 'NONE', #1551, #880 ) ;
#9116 = DIRECTION ( 'NONE',  ( -0.5000000000000073275, 0.000000000000000000, -0.8660254037844344888 ) ) ;
#9117 = LINE ( 'NONE', #10946, #7070 ) ;
#9118 = ORIENTED_EDGE ( 'NONE', *, *, #2258, .T. ) ;
#9119 = VECTOR ( 'NONE', #6442, 1000.000000000000000 ) ;
#9120 = ORIENTED_EDGE ( 'NONE', *, *, #2395, .T. ) ;
#9121 = ORIENTED_EDGE ( 'NONE', *, *, #5600, .F. ) ;
#9122 = VECTOR ( 'NONE', #9426, 1000.000000000000227 ) ;
#9123 = PRODUCT_DEFINITION_CONTEXT ( 'detailed design', #8794, 'design' ) ;
#9124 = CARTESIAN_POINT ( 'NONE',  ( 24.62111388750000174, 0.3937499990440845310, 0.000000000000000000 ) ) ;
#9125 = CARTESIAN_POINT ( 'NONE',  ( -10.19839929293507552, 1.906249999044084431, 24.62111388749999463 ) ) ;
#9126 = DIRECTION ( 'NONE',  ( -0.000000000000000000, 1.000000000000000000, -0.000000000000000000 ) ) ;
#9127 = LINE ( 'NONE', #5937, #8451 ) ;
#9128 = CARTESIAN_POINT ( 'NONE',  ( 10.19839929293506486, 1.031249999044084653, 24.62111388749999819 ) ) ;
#9129 = DIRECTION ( 'NONE',  ( 0.000000000000000000, 1.000000000000000000, 0.000000000000000000 ) ) ;
#9130 = AXIS2_PLACEMENT_3D ( 'NONE', #1191, #8907, #10465 ) ;
#9131 = CARTESIAN_POINT ( 'NONE',  ( 1.507608415688466075E-15, 1.468749999044084431, -24.62111388750000174 ) ) ;
#9132 = DIRECTION ( 'NONE',  ( 0.000000000000000000, 1.000000000000000000, -0.000000000000000000 ) ) ;
#9133 = EDGE_LOOP ( 'NONE', ( #596, #8549, #4469, #10310, #2000, #9977, #3622, #6643, #8290, #5331, #6608, #9912, #9923 ) ) ;
#9134 = ORIENTED_EDGE ( 'NONE', *, *, #9372, .F. ) ;
#9135 = EDGE_LOOP ( 'NONE', ( #2916, #6830 ) ) ;
#9136 = APPLICATION_CONTEXT ( 'automotive_design' ) ;
#9137 = EDGE_LOOP ( 'NONE', ( #8428, #9932, #6651, #6015 ) ) ;
#9138 = VECTOR ( 'NONE', #8571, 1000.000000000000000 ) ;
#9139 = PLANE ( 'NONE',  #5697 ) ;
#9140 = CARTESIAN_POINT ( 'NONE',  ( -6.999999999999997335, 20.00000000000000355, -7.332110811570577522E-14 ) ) ;
#9141 = DIRECTION ( 'NONE',  ( 0.000000000000000000, 0.000000000000000000, -1.000000000000000000 ) ) ;
#9142 = ADVANCED_BREP_SHAPE_REPRESENTATION ( '', ( #3360, #7040 ), #7026 ) ;
#9143 = EDGE_CURVE ( 'NONE', #8513, #1851, #8150, .T. ) ;
#9144 = CARTESIAN_POINT ( 'NONE',  ( 1.530808498934191521E-15, 1.862499998088169129, -25.00000000000000000 ) ) ;
#9145 = EDGE_CURVE ( 'NONE', #5496, #6765, #8566, .T. ) ;
#9146 = CARTESIAN_POINT ( 'NONE',  ( 12.19759864389371629, 5.000000000000001776, 21.50133847031806411 ) ) ;
#9147 = ADVANCED_FACE ( 'NONE', ( #8448 ), #926, .T. ) ;
#9148 = ORIENTED_EDGE ( 'NONE', *, *, #1938, .T. ) ;
#9149 = CARTESIAN_POINT ( 'NONE',  ( 8.499999999999998224, 92.59807621135333022, -5.000000000000000000 ) ) ;
#9150 = CARTESIAN_POINT ( 'NONE',  ( -7.874999999999821476, -0.001000000000001000089, 13.63990010960501031 ) ) ;
#9151 = PLANE ( 'NONE',  #8105 ) ;
#9152 = PRODUCT_CONTEXT ( 'NONE', #9576, 'mechanical' ) ;
#9153 = DIRECTION ( 'NONE',  ( -1.000000000000000000, 0.000000000000000000, 0.000000000000000000 ) ) ;
#9154 = ORIENTED_EDGE ( 'NONE', *, *, #3124, .T. ) ;
#9155 = DIRECTION ( 'NONE',  ( 0.000000000000000000, -0.000000000000000000, 1.000000000000000000 ) ) ;
#9156 = EDGE_CURVE ( 'NONE', #7557, #10846, #5504, .T. ) ;
#9157 = CARTESIAN_POINT ( 'NONE',  ( -24.62111388750000174, 2.718749999044084653, -3.015216831376932151E-15 ) ) ;
#9158 = ORIENTED_EDGE ( 'NONE', *, *, #10223, .T. ) ;
#9159 = ORIENTED_EDGE ( 'NONE', *, *, #3967, .T. ) ;
#9160 = EDGE_CURVE ( 'NONE', #1567, #3209, #9613, .T. ) ;
#9161 = VECTOR ( 'NONE', #4085, 1000.000000000000000 ) ;
#9162 = VECTOR ( 'NONE', #7403, 1000.000000000000000 ) ;
#9163 = CARTESIAN_POINT ( 'NONE',  ( -10.35533905932737575, 4.924999998088169129, -25.00000000000000000 ) ) ;
#9164 = DIRECTION ( 'NONE',  ( 0.4999999999999951705, 0.000000000000000000, -0.8660254037844413721 ) ) ;
#9165 = CARTESIAN_POINT ( 'NONE',  ( -17.40975659021752975, 0.5937499990440846531, -17.40975659021752975 ) ) ;
#9166 = CARTESIAN_POINT ( 'NONE',  ( 14.00000000000000533, 0.000000000000000000, 0.000000000000000000 ) ) ;
#9167 = ORIENTED_EDGE ( 'NONE', *, *, #8980, .T. ) ;
#9168 = CARTESIAN_POINT ( 'NONE',  ( 29.32100596316561081, 99.46396820659043669, -5.000000000000000000 ) ) ;
#9169 = FACE_OUTER_BOUND ( 'NONE', #10044, .T. ) ;
#9170 = DIRECTION ( 'NONE',  ( 0.000000000000000000, -1.000000000000000000, 0.000000000000000000 ) ) ;
#9171 = DIRECTION ( 'NONE',  ( -0.6123724356957870318, 0.3535533905932747301, -0.7071067811865536790 ) ) ;
#9172 = CARTESIAN_POINT ( 'NONE',  ( -3.433012701892259155, 10.00000000000000355, 4.946152422706602714 ) ) ;
#9173 = AXIS2_PLACEMENT_3D ( 'NONE', #8147, #7117, #10482 ) ;
#9174 = VERTEX_POINT ( 'NONE', #2045 ) ;
#9175 = EDGE_LOOP ( 'NONE', ( #4827, #9844 ) ) ;
#9176 = CIRCLE ( 'NONE', #7236, 2.999999999999996447 ) ;
#9177 = PRESENTATION_LAYER_ASSIGNMENT (  '', '', ( #10251 ) ) ;
#9178 = CARTESIAN_POINT ( 'NONE',  ( -17.40975659021753330, 3.018749999044084475, 17.40975659021752975 ) ) ;
#9179 = CARTESIAN_POINT ( 'NONE',  ( 24.62111388750000174, 0.2187499990440845699, 0.000000000000000000 ) ) ;
#9180 = FILL_AREA_STYLE_COLOUR ( '', #3678 ) ;
#9181 = ORIENTED_EDGE ( 'NONE', *, *, #3491, .T. ) ;
#9182 = CARTESIAN_POINT ( 'NONE',  ( -10.35533905932736687, 1.924999998088168907, -25.00000000000000711 ) ) ;
#9183 = LINE ( 'NONE', #2755, #2689 ) ;
#9184 = CARTESIAN_POINT ( 'NONE',  ( 0.000000000000000000, 82.00000000000000000, 0.000000000000000000 ) ) ;
#9185 = CARTESIAN_POINT ( 'NONE',  ( 17.40975659021752975, 1.343749999044084653, -17.40975659021752975 ) ) ;
#9186 = DIRECTION ( 'NONE',  ( 0.000000000000000000, 1.000000000000000000, -1.502202555303642096E-16 ) ) ;
#9187 = ORIENTED_EDGE ( 'NONE', *, *, #7494, .T. ) ;
#9188 = ORIENTED_EDGE ( 'NONE', *, *, #3817, .F. ) ;
#9189 = AXIS2_PLACEMENT_3D ( 'NONE', #79, #7480, #2391 ) ;
#9190 = EDGE_LOOP ( 'NONE', ( #2982, #5797, #9250, #10731 ) ) ;
#9191 = DIRECTION ( 'NONE',  ( -0.5000000000000103251, 0.000000000000000000, -0.8660254037844327124 ) ) ;
#9192 = DIRECTION ( 'NONE',  ( 0.000000000000000000, -2.775557561562887961E-17, -1.000000000000000000 ) ) ;
#9193 = CARTESIAN_POINT ( 'NONE',  ( 25.00000000000000000, 5.000000000000000000, 0.000000000000000000 ) ) ;
#9194 = DIRECTION ( 'NONE',  ( -0.000000000000000000, -1.000000000000000000, -0.000000000000000000 ) ) ;
#9195 = CARTESIAN_POINT ( 'NONE',  ( 15.18771902014174735, 5.000000000000000888, 19.59342933435411993 ) ) ;
#9196 = AXIS2_PLACEMENT_3D ( 'NONE', #10093, #874, #5788 ) ;
#9197 = ORIENTED_EDGE ( 'NONE', *, *, #10181, .T. ) ;
#9198 = AXIS2_PLACEMENT_3D ( 'NONE', #8424, #10029, #4965 ) ;
#9199 = ADVANCED_FACE ( 'NONE', ( #10540 ), #7952, .F. ) ;
#9200 = CARTESIAN_POINT ( 'NONE',  ( 10.35533905932742016, 4.812499999999999112, 24.99999999999996447 ) ) ;
#9201 = LINE ( 'NONE', #2304, #6849 ) ;
#9202 = CARTESIAN_POINT ( 'NONE',  ( -4.592425496802574367E-15, 1.362499998088169129, 25.00000000000000000 ) ) ;
#9203 = TOROIDAL_SURFACE ( 'NONE', #4108, 5.100000000000000533, 0.1000000000000001582 ) ;
#9204 = APPLICATION_PROTOCOL_DEFINITION ( 'draft international standard', 'automotive_design', 1998, #4853 ) ;
#9205 = CIRCLE ( 'NONE', #10631, 12.77350269189627063 ) ;
#9206 = PLANE ( 'NONE',  #8527 ) ;
#9207 = CARTESIAN_POINT ( 'NONE',  ( -25.00000000000000000, 1.437500000000000000, -10.35533905932738108 ) ) ;
#9208 = CARTESIAN_POINT ( 'NONE',  ( -4.522825247065398226E-15, 2.968749999044084653, 24.62111388750000174 ) ) ;
#9209 = ADVANCED_FACE ( 'NONE', ( #7129 ), #5223, .F. ) ;
#9210 = VECTOR ( 'NONE', #1856, 1000.000000000000227 ) ;
#9211 = ORIENTED_EDGE ( 'NONE', *, *, #10780, .T. ) ;
#9212 = AXIS2_PLACEMENT_3D ( 'NONE', #3710, #2754, #7091 ) ;
#9213 = ORIENTED_EDGE ( 'NONE', *, *, #7935, .F. ) ;
#9214 = AXIS2_PLACEMENT_3D ( 'NONE', #8777, #1219, #4647 ) ;
#9215 = EDGE_CURVE ( 'NONE', #2700, #1860, #7627, .T. ) ;
#9216 = CARTESIAN_POINT ( 'NONE',  ( 1.507608415688466075E-15, 4.643749999044084475, -24.62111388750000174 ) ) ;
#9217 = LINE ( 'NONE', #4372, #10759 ) ;
#9218 = CARTESIAN_POINT ( 'NONE',  ( -4.522825247065398226E-15, 1.968749999044084653, 24.62111388750000174 ) ) ;
#9219 = LINE ( 'NONE', #1662, #10274 ) ;
#9220 = VERTEX_POINT ( 'NONE', #961 ) ;
#9221 = DIRECTION ( 'NONE',  ( -1.000000000000000000, 0.000000000000000000, -0.000000000000000000 ) ) ;
#9222 = CARTESIAN_POINT ( 'NONE',  ( -4.592425496802574367E-15, 1.362499998088169129, 25.00000000000000000 ) ) ;
#9223 = DIRECTION ( 'NONE',  ( 1.000000000000000000, 0.000000000000000000, 0.000000000000000000 ) ) ;
#9224 = CIRCLE ( 'NONE', #1141, 6.975000000000008527 ) ;
#9225 = DIRECTION ( 'NONE',  ( 0.000000000000000000, 0.000000000000000000, -1.000000000000000000 ) ) ;
#9226 = DIRECTION ( 'NONE',  ( 1.000000000000000000, 0.000000000000000000, 0.000000000000000000 ) ) ;
#9227 = EDGE_CURVE ( 'NONE', #9763, #2965, #397, .T. ) ;
#9228 = AXIS2_PLACEMENT_3D ( 'NONE', #2449, #6614, #8254 ) ;
#9229 = VERTEX_POINT ( 'NONE', #2088 ) ;
#9230 = VERTEX_POINT ( 'NONE', #8827 ) ;
#9231 = VERTEX_POINT ( 'NONE', #1268 ) ;
#9232 = DIRECTION ( 'NONE',  ( -0.000000000000000000, -1.000000000000000000, -0.000000000000000000 ) ) ;
#9233 = CARTESIAN_POINT ( 'NONE',  ( 24.62111388749999463, 1.331249999044084475, 10.19839929293507730 ) ) ;
#9234 = CARTESIAN_POINT ( 'NONE',  ( -17.40975659021753330, 0.8437499990440846531, 17.40975659021752975 ) ) ;
#9235 = CARTESIAN_POINT ( 'NONE',  ( -11.92163336986823374, 7.781088913245559624, -6.305607966084005866 ) ) ;
#9236 = EDGE_CURVE ( 'NONE', #3039, #5184, #1272, .T. ) ;
#9237 = DIRECTION ( 'NONE',  ( 0.5000000000000101030, 0.000000000000000000, -0.8660254037844328234 ) ) ;
#9238 = CARTESIAN_POINT ( 'NONE',  ( 17.67766952966368521, 4.487499998088169129, 17.67766952966369232 ) ) ;
#9239 = CARTESIAN_POINT ( 'NONE',  ( -24.62111388750000174, 3.656249999044084653, -10.19839929293506131 ) ) ;
#9240 = CARTESIAN_POINT ( 'NONE',  ( 6.982120021884465899, 19.03096903053429401, 0.5000000000000244249 ) ) ;
#9241 = VERTEX_POINT ( 'NONE', #7746 ) ;
#9242 = ORIENTED_EDGE ( 'NONE', *, *, #5768, .T. ) ;
#9243 = ORIENTED_EDGE ( 'NONE', *, *, #2033, .T. ) ;
#9244 = ORIENTED_EDGE ( 'NONE', *, *, #3926, .F. ) ;
#9245 = DIRECTION ( 'NONE',  ( 0.000000000000000000, 0.000000000000000000, -1.000000000000000000 ) ) ;
#9246 = CARTESIAN_POINT ( 'NONE',  ( 3.499999999999963141, 20.00000000000000355, 6.062177826491089050 ) ) ;
#9247 = DIRECTION ( 'NONE',  ( 0.000000000000000000, 0.000000000000000000, 1.000000000000000000 ) ) ;
#9248 = CARTESIAN_POINT ( 'NONE',  ( 0.000000000000000000, 1.000000000000002220, -0.5773502691896270633 ) ) ;
#9249 = CARTESIAN_POINT ( 'NONE',  ( 6.982120021884465899, 10.00000000000000355, 0.5000000000000244249 ) ) ;
#9250 = ORIENTED_EDGE ( 'NONE', *, *, #7395, .F. ) ;
#9251 = CARTESIAN_POINT ( 'NONE',  ( 7.856406460551036197, 93.00000000000001421, 5.000000000000000000 ) ) ;
#9252 = DIRECTION ( 'NONE',  ( 0.000000000000000000, -0.000000000000000000, -1.000000000000000000 ) ) ;
#9253 = CARTESIAN_POINT ( 'NONE',  ( -25.00000000000001066, 4.562500000000001776, 10.35533905932737397 ) ) ;
#9254 = DIRECTION ( 'NONE',  ( -1.000000000000000000, 0.000000000000000000, 0.000000000000000000 ) ) ;
#9255 = VERTEX_POINT ( 'NONE', #1779 ) ;
#9256 = DIRECTION ( 'NONE',  ( -0.000000000000000000, -1.000000000000000000, -0.000000000000000000 ) ) ;
#9257 = CARTESIAN_POINT ( 'NONE',  ( 0.000000000000000000, -58.00000000000000000, 0.000000000000000000 ) ) ;
#9258 = CARTESIAN_POINT ( 'NONE',  ( -6.982120021884473005, 19.03096903053431888, 0.4999999999999268363 ) ) ;
#9259 = LINE ( 'NONE', #6139, #8789 ) ;
#9260 = EDGE_CURVE ( 'NONE', #9521, #3157, #2664, .T. ) ;
#9261 = ORIENTED_EDGE ( 'NONE', *, *, #4682, .F. ) ;
#9262 = ORIENTED_EDGE ( 'NONE', *, *, #2406, .F. ) ;
#9263 = ADVANCED_FACE ( 'NONE', ( #9711 ), #9330, .F. ) ;
#9264 = CARTESIAN_POINT ( 'NONE',  ( 24.62111388750000174, 2.456249999044084475, -10.19839929293505776 ) ) ;
#9265 = LINE ( 'NONE', #8440, #2817 ) ;
#9266 = CARTESIAN_POINT ( 'NONE',  ( -10.35533905932739174, 1.299999998088168907, 24.99999999999999289 ) ) ;
#9267 = DIRECTION ( 'NONE',  ( -3.708321773340234242E-15, 0.000000000000000000, -1.000000000000000000 ) ) ;
#9268 = ORIENTED_EDGE ( 'NONE', *, *, #5846, .F. ) ;
#9269 = LINE ( 'NONE', #3471, #8450 ) ;
#9270 = SURFACE_SIDE_STYLE ('',( #785 ) ) ;
#9271 = DIRECTION ( 'NONE',  ( 0.000000000000000000, -2.775557561562888270E-17, -1.000000000000000000 ) ) ;
#9272 = CARTESIAN_POINT ( 'NONE',  ( -13.63990010960498367, 28.00000000000000000, -7.874999999999870326 ) ) ;
#9273 = PLANE ( 'NONE',  #7614 ) ;
#9274 = FACE_OUTER_BOUND ( 'NONE', #10611, .T. ) ;
#9275 = EDGE_CURVE ( 'NONE', #6044, #1816, #4326, .T. ) ;
#9276 = EDGE_CURVE ( 'NONE', #10743, #2139, #7432, .T. ) ;
#9277 = EDGE_CURVE ( 'NONE', #5812, #120, #9807, .T. ) ;
#9278 = ORIENTED_EDGE ( 'NONE', *, *, #3616, .T. ) ;
#9279 = EDGE_LOOP ( 'NONE', ( #6679, #7134, #226, #9654 ) ) ;
#9280 = EDGE_CURVE ( 'NONE', #8862, #5226, #10652, .T. ) ;
#9281 = DIRECTION ( 'NONE',  ( 0.000000000000000000, -0.9396926207859082059, -0.3420201433256694901 ) ) ;
#9282 = CARTESIAN_POINT ( 'NONE',  ( 17.40975659021752620, 5.268749999044085364, 17.40975659021753330 ) ) ;
#9283 = FACE_OUTER_BOUND ( 'NONE', #4544, .T. ) ;
#9284 =( BOUNDED_SURFACE ( )  B_SPLINE_SURFACE ( 1, 2, ( 
 ( #9179, #6649, #6769, #1617, #4003, #624, #8358, #7476, #9955, #3250, #9234, #10069, #681, #2334, #4056, #5060, #5718, #7527, #799, #4165, #8191, #10852, #10906, #2484, #5881, #2386, #1678, #9125, #8404, #1558, #847, #4215, #4886, #7578, #7356, #3145, #6541, #8237, #10179, #249, #4336, #972, #6110, #3607, #2597, #10301, #6995, #6879, #6942, #7755, #9286, #2714, #5991, #3489, #187, #10351, #7640, #128, #1903, #8458, #3430, #3547, #9471, #299, #1142, #9410, #5284, #4457, #2764, #8632, #10237, #6163, #8695, #1081, #1024, #7816, #7699, #4393, #2652, #5232, #9527 ),
 ( #8575, #1964, #5337, #4521, #7876, #6050, #3664, #75, #9346, #10129, #2541, #5934, #1849, #1729, #5107, #907, #4275, #6822, #1790, #5171, #8521, #10516, #6221, #458, #2023, #5595, #7195, #7101, #3828, #10563, #8126, #2973, #8751, #5394, #6378, #9684, #3781, #8027, #3032, #3878, #5437, #10464, #8798, #9782, #2879, #1340, #9732, #2162, #6275, #4570, #4769, #5547, #9582, #6433, #4678, #407, #9632, #2060, #1189, #4720, #1237, #4620, #7923, #8905, #8073, #506, #7244, #10616, #7152, #2214, #7975, #8955, #2921, #6321, #1384, #3723, #555, #2107, #351, #7047, #10405 ) ),
 .UNSPECIFIED., .F., .F., .F. ) 
 B_SPLINE_SURFACE_WITH_KNOTS ( ( 2, 2 ),
 ( 3, 2, 2, 2, 2, 2, 2, 2, 2, 2, 2, 2, 2, 2, 2, 2, 2, 2, 2, 2, 2, 2, 2, 2, 2, 2, 2, 2, 2, 2, 2, 2, 2, 2, 2, 2, 2, 2, 2, 2, 3 ),
 ( 0.000000000000000000, 1.000000000000000000 ),
 ( 0.000000000000000000, 0.02500000000000000139, 0.05000000000000000278, 0.07499999999999999722, 0.1000000000000000056, 0.1250000000000000000, 0.1499999999999999944, 0.1749999999999999889, 0.2000000000000000111, 0.2250000000000000056, 0.2500000000000000000, 0.2750000000000000222, 0.2999999999999999889, 0.3250000000000000111, 0.3499999999999999778, 0.3750000000000000000, 0.4000000000000000222, 0.4249999999999999889, 0.4500000000000000111, 0.4749999999999999778, 0.5000000000000000000, 0.5250000000000000222, 0.5500000000000000444, 0.5749999999999999556, 0.5999999999999999778, 0.6250000000000000000, 0.6500000000000000222, 0.6750000000000000444, 0.6999999999999999556, 0.7249999999999999778, 0.7500000000000000000, 0.7750000000000000222, 0.8000000000000000444, 0.8249999999999999556, 0.8499999999999999778, 0.8750000000000000000, 0.9000000000000000222, 0.9250000000000000444, 0.9499999999999999556, 0.9749999999999999778, 1.000000000000000000 ),
 .UNSPECIFIED. ) 
 GEOMETRIC_REPRESENTATION_ITEM ( )  RATIONAL_B_SPLINE_SURFACE ( (
 ( 1.000000000000000000, 0.9238795325112867385, 1.000000000000000000, 0.9238795325112867385, 1.000000000000000000, 0.9238795325112867385, 1.000000000000000000, 0.9238795325112867385, 1.000000000000000000, 0.9238795325112867385, 1.000000000000000000, 0.9238795325112867385, 1.000000000000000000, 0.9238795325112867385, 1.000000000000000000, 0.9238795325112867385, 1.000000000000000000, 0.9238795325112867385, 1.000000000000000000, 0.9238795325112867385, 1.000000000000000000, 0.9238795325112867385, 1.000000000000000000, 0.9238795325112867385, 1.000000000000000000, 0.9238795325112867385, 1.000000000000000000, 0.9238795325112867385, 1.000000000000000000, 0.9238795325112867385, 1.000000000000000000, 0.9238795325112867385, 1.000000000000000000, 0.9238795325112867385, 1.000000000000000000, 0.9238795325112867385, 1.000000000000000000, 0.9238795325112867385, 1.000000000000000000, 0.9238795325112867385, 1.000000000000000000, 0.9238795325112867385, 1.000000000000000000, 0.9238795325112867385, 1.000000000000000000, 0.9238795325112867385, 1.000000000000000000, 0.9238795325112867385, 1.000000000000000000, 0.9238795325112867385, 1.000000000000000000, 0.9238795325112867385, 1.000000000000000000, 0.9238795325112867385, 1.000000000000000000, 0.9238795325112867385, 1.000000000000000000, 0.9238795325112867385, 1.000000000000000000, 0.9238795325112867385, 1.000000000000000000, 0.9238795325112867385, 1.000000000000000000, 0.9238795325112867385, 1.000000000000000000, 0.9238795325112867385, 1.000000000000000000, 0.9238795325112867385, 1.000000000000000000, 0.9238795325112867385, 1.000000000000000000, 0.9238795325112867385, 1.000000000000000000, 0.9238795325112867385, 1.000000000000000000, 0.9238795325112867385, 1.000000000000000000, 0.9238795325112867385, 1.000000000000000000, 0.9238795325112867385, 1.000000000000000000),
 ( 1.000000000000000000, 0.9238795325112867385, 1.000000000000000000, 0.9238795325112867385, 1.000000000000000000, 0.9238795325112867385, 1.000000000000000000, 0.9238795325112867385, 1.000000000000000000, 0.9238795325112867385, 1.000000000000000000, 0.9238795325112867385, 1.000000000000000000, 0.9238795325112867385, 1.000000000000000000, 0.9238795325112867385, 1.000000000000000000, 0.9238795325112867385, 1.000000000000000000, 0.9238795325112867385, 1.000000000000000000, 0.9238795325112867385, 1.000000000000000000, 0.9238795325112867385, 1.000000000000000000, 0.9238795325112867385, 1.000000000000000000, 0.9238795325112867385, 1.000000000000000000, 0.9238795325112867385, 1.000000000000000000, 0.9238795325112867385, 1.000000000000000000, 0.9238795325112867385, 1.000000000000000000, 0.9238795325112867385, 1.000000000000000000, 0.9238795325112867385, 1.000000000000000000, 0.9238795325112867385, 1.000000000000000000, 0.9238795325112867385, 1.000000000000000000, 0.9238795325112867385, 1.000000000000000000, 0.9238795325112867385, 1.000000000000000000, 0.9238795325112867385, 1.000000000000000000, 0.9238795325112867385, 1.000000000000000000, 0.9238795325112867385, 1.000000000000000000, 0.9238795325112867385, 1.000000000000000000, 0.9238795325112867385, 1.000000000000000000, 0.9238795325112867385, 1.000000000000000000, 0.9238795325112867385, 1.000000000000000000, 0.9238795325112867385, 1.000000000000000000, 0.9238795325112867385, 1.000000000000000000, 0.9238795325112867385, 1.000000000000000000, 0.9238795325112867385, 1.000000000000000000, 0.9238795325112867385, 1.000000000000000000, 0.9238795325112867385, 1.000000000000000000, 0.9238795325112867385, 1.000000000000000000, 0.9238795325112867385, 1.000000000000000000, 0.9238795325112867385, 1.000000000000000000, 0.9238795325112867385, 1.000000000000000000) ) ) 
 REPRESENTATION_ITEM ( '' )  SURFACE ( )  );
#9285 = CARTESIAN_POINT ( 'NONE',  ( 24.62111388750000174, 1.393749999044084475, 0.000000000000000000 ) ) ;
#9286 = CARTESIAN_POINT ( 'NONE',  ( 17.40975659021752975, 3.343749999044085097, -17.40975659021752975 ) ) ;
#9287 = DIRECTION ( 'NONE',  ( -0.000000000000000000, 1.000000000000000000, -0.000000000000000000 ) ) ;
#9288 = CARTESIAN_POINT ( 'NONE',  ( 6.062177826491051746, 20.00000000000000355, 3.500000000000027089 ) ) ;
#9289 = CARTESIAN_POINT ( 'NONE',  ( 2.500000000000000444, 1.000000000000002220, -0.5773502691896270633 ) ) ;
#9290 = CARTESIAN_POINT ( 'NONE',  ( 1.530808498934191521E-15, 1.250000000000000000, -25.00000000000000000 ) ) ;
#9291 = ADVANCED_FACE ( 'NONE', ( #3107, #4022 ), #4804, .T. ) ;
#9292 = DIRECTION ( 'NONE',  ( -0.000000000000000000, 1.000000000000000000, 0.000000000000000000 ) ) ;
#9293 = VERTEX_POINT ( 'NONE', #10748 ) ;
#9294 = CIRCLE ( 'NONE', #1205, 2.999999999999999112 ) ;
#9295 = ORIENTED_EDGE ( 'NONE', *, *, #855, .T. ) ;
#9296 = ORIENTED_EDGE ( 'NONE', *, *, #3148, .T. ) ;
#9297 = ORIENTED_EDGE ( 'NONE', *, *, #9624, .T. ) ;
#9298 = CARTESIAN_POINT ( 'NONE',  ( 6.580127018922133253, 10.00000000000000355, 11.12916512459891116 ) ) ;
#9299 = ADVANCED_FACE ( 'NONE', ( #6560 ), #5680, .F. ) ;
#9300 = CIRCLE ( 'NONE', #2587, 5.000000000000005329 ) ;
#9301 = DIRECTION ( 'NONE',  ( 0.000000000000000000, 0.000000000000000000, 1.000000000000000000 ) ) ;
#9302 = ORIENTED_EDGE ( 'NONE', *, *, #10388, .F. ) ;
#9303 = CARTESIAN_POINT ( 'NONE',  ( 17.67766952966369232, 2.125000000000000000, -17.67766952966369232 ) ) ;
#9304 = DIRECTION ( 'NONE',  ( -0.000000000000000000, 1.000000000000000000, -0.000000000000000000 ) ) ;
#9305 = CARTESIAN_POINT ( 'NONE',  ( -4.592425496802574367E-15, 3.750000000000000000, 25.00000000000000000 ) ) ;
#9306 = CARTESIAN_POINT ( 'NONE',  ( 7.875000000000019540, 28.00000000000000000, 13.63990010960489840 ) ) ;
#9307 = CARTESIAN_POINT ( 'NONE',  ( 22.95776900584396074, 5.000000000000000000, 9.642149850605726158 ) ) ;
#9308 = AXIS2_PLACEMENT_3D ( 'NONE', #2436, #5760, #1506 ) ;
#9309 = VERTEX_POINT ( 'NONE', #2299 ) ;
#9310 = VECTOR ( 'NONE', #4243, 1000.000000000000000 ) ;
#9311 = VERTEX_POINT ( 'NONE', #9760 ) ;
#9312 = DIRECTION ( 'NONE',  ( 0.000000000000000000, 0.000000000000000000, 1.000000000000000000 ) ) ;
#9313 = CARTESIAN_POINT ( 'NONE',  ( -17.67766952966368876, 4.375000000000000000, -17.67766952966369232 ) ) ;
#9314 = CARTESIAN_POINT ( 'NONE',  ( 3.957930336368489021E-15, -0.001000000000001000089, 19.75000000000000000 ) ) ;
#9315 = PLANE ( 'NONE',  #3525 ) ;
#9316 = CARTESIAN_POINT ( 'NONE',  ( -3.785909150702975179, 19.34316356887877930, -5.890223162633914988 ) ) ;
#9317 = ORIENTED_EDGE ( 'NONE', *, *, #1008, .F. ) ;
#9318 = CARTESIAN_POINT ( 'NONE',  ( 5.890223162633874132, 19.34316356887878641, -3.785909150703038240 ) ) ;
#9319 = CARTESIAN_POINT ( 'NONE',  ( -17.40975659021753330, 4.843749999044083765, 17.40975659021752975 ) ) ;
#9320 = VERTEX_POINT ( 'NONE', #8929 ) ;
#9321 = CARTESIAN_POINT ( 'NONE',  ( 10.19839929293506486, 4.206249999044084475, 24.62111388749999819 ) ) ;
#9322 = FACE_OUTER_BOUND ( 'NONE', #7228, .T. ) ;
#9323 = CARTESIAN_POINT ( 'NONE',  ( -4.592425496802574367E-15, 2.750000000000000000, 25.00000000000000000 ) ) ;
#9324 = CARTESIAN_POINT ( 'NONE',  ( -19.75000000000003197, 28.00000000000000000, -2.999999999999789946 ) ) ;
#9325 = ORIENTED_EDGE ( 'NONE', *, *, #658, .T. ) ;
#9326 = CARTESIAN_POINT ( 'NONE',  ( -25.00000000000001066, 1.174999998088169351, 10.35533905932737397 ) ) ;
#9327 =( NAMED_UNIT ( * ) PLANE_ANGLE_UNIT ( ) SI_UNIT ( $, .RADIAN. ) );
#9328 = DIRECTION ( 'NONE',  ( 0.000000000000000000, 0.8660254037844385966, -0.4999999999999998890 ) ) ;
#9329 = CARTESIAN_POINT ( 'NONE',  ( 10.35533905932737930, 1.799999998088168907, -25.00000000000000000 ) ) ;
#9330 = CYLINDRICAL_SURFACE ( 'NONE', #9733, 2.999999999999997335 ) ;
#9331 = LINE ( 'NONE', #5755, #3705 ) ;
#9332 = PRODUCT_DEFINITION_SHAPE ( 'NONE', 'NONE',  #3451 ) ;
#9333 = VECTOR ( 'NONE', #10166, 1000.000000000000000 ) ;
#9334 = EDGE_LOOP ( 'NONE', ( #3193, #4253, #10862, #5180 ) ) ;
#9335 = VECTOR ( 'NONE', #10000, 1000.000000000000000 ) ;
#9336 = ORIENTED_EDGE ( 'NONE', *, *, #9156, .T. ) ;
#9337 = VERTEX_POINT ( 'NONE', #4861 ) ;
#9338 = EDGE_LOOP ( 'NONE', ( #3019, #7340, #6595, #10790, #7354, #2558 ) ) ;
#9339 = ORIENTED_EDGE ( 'NONE', *, *, #3618, .T. ) ;
#9340 = FACE_OUTER_BOUND ( 'NONE', #3827, .T. ) ;
#9341 = CARTESIAN_POINT ( 'NONE',  ( -4.522825247065398226E-15, 3.143749999044084475, 24.62111388750000174 ) ) ;
#9342 = DIRECTION ( 'NONE',  ( 0.000000000000000000, 2.775557561562887961E-17, 1.000000000000000000 ) ) ;
#9343 = EDGE_CURVE ( 'NONE', #4087, #3378, #3219, .T. ) ;
#9344 = ADVANCED_FACE ( 'NONE', ( #3063 ), #7221, .F. ) ;
#9345 = CARTESIAN_POINT ( 'NONE',  ( 10.19839929293505953, 2.581249999044084475, -24.62111388750000174 ) ) ;
#9346 = CARTESIAN_POINT ( 'NONE',  ( -25.00000000000000000, 0.5000000000000000000, -3.061616997868383043E-15 ) ) ;
#9347 = DIRECTION ( 'NONE',  ( -0.000000000000000000, 1.000000000000000000, -0.000000000000000000 ) ) ;
#9348 = AXIS2_PLACEMENT_3D ( 'NONE', #5528, #8894, #9621 ) ;
#9349 = CIRCLE ( 'NONE', #5132, 5.000000000000005329 ) ;
#9350 = ORIENTED_EDGE ( 'NONE', *, *, #6588, .F. ) ;
#9351 = CARTESIAN_POINT ( 'NONE',  ( 2.500000000000000444, 1.000000000000001998, 0.5773502691896277295 ) ) ;
#9352 = FACE_BOUND ( 'NONE', #2444, .T. ) ;
#9353 = DIRECTION ( 'NONE',  ( -0.000000000000000000, 1.000000000000000000, 0.000000000000000000 ) ) ;
#9354 = CARTESIAN_POINT ( 'NONE',  ( -10.19839929293505776, 4.531249999044084653, -24.62111388750000174 ) ) ;
#9355 = CARTESIAN_POINT ( 'NONE',  ( 13.63990010960487353, -0.001000000000001000089, -4.875000000000070166 ) ) ;
#9356 = EDGE_CURVE ( 'NONE', #5164, #1987, #6457, .T. ) ;
#9357 = ORIENTED_EDGE ( 'NONE', *, *, #5404, .F. ) ;
#9358 = VERTEX_POINT ( 'NONE', #2195 ) ;
#9359 = ORIENTED_EDGE ( 'NONE', *, *, #7073, .T. ) ;
#9360 = CIRCLE ( 'NONE', #898, 5.000000000000004441 ) ;
#9361 = MECHANICAL_DESIGN_GEOMETRIC_PRESENTATION_REPRESENTATION (  '', ( #540 ), #8472 ) ;
#9362 =( BOUNDED_CURVE ( )  B_SPLINE_CURVE ( 3, ( #2050, #4554, #2907, #8836 ),
 .UNSPECIFIED., .F., .F. ) 
 B_SPLINE_CURVE_WITH_KNOTS ( ( 4, 4 ),
 ( 2.284520705739657487, 2.356010155625178015 ),
 .UNSPECIFIED. ) 
 CURVE ( )  GEOMETRIC_REPRESENTATION_ITEM ( )  RATIONAL_B_SPLINE_CURVE ( ( 1.000000000000000000, 0.9995741502243209453, 0.9995741502243209453, 1.000000000000000000 ) ) 
 REPRESENTATION_ITEM ( '' )  );
#9363 = CARTESIAN_POINT ( 'NONE',  ( -10.00000000000000000, 90.00000000000001421, 5.000000000000000000 ) ) ;
#9364 = EDGE_CURVE ( 'NONE', #689, #9550, #9914, .T. ) ;
#9365 = CARTESIAN_POINT ( 'NONE',  ( -25.00000000000000000, 4.112499998088169129, -3.061616997868383043E-15 ) ) ;
#9366 = LINE ( 'NONE', #6724, #2175 ) ;
#9367 = DIRECTION ( 'NONE',  ( 0.8660254037844450359, 0.000000000000000000, -0.4999999999999888978 ) ) ;
#9368 = AXIS2_PLACEMENT_3D ( 'NONE', #517, #7207, #10576 ) ;
#9369 = CARTESIAN_POINT ( 'NONE',  ( 0.000000000000000000, 10.00000000000000355, 0.000000000000000000 ) ) ;
#9370 = DIRECTION ( 'NONE',  ( -0.000000000000000000, 1.000000000000000000, -0.000000000000000000 ) ) ;
#9371 = CARTESIAN_POINT ( 'NONE',  ( 24.95478587032620865, 5.000000000000001776, 1.418225997825871554 ) ) ;
#9372 = EDGE_CURVE ( 'NONE', #10596, #448, #7434, .T. ) ;
#9373 = CIRCLE ( 'NONE', #10787, 12.77350269189627063 ) ;
#9374 = ORIENTED_EDGE ( 'NONE', *, *, #8393, .F. ) ;
#9375 = ORIENTED_EDGE ( 'NONE', *, *, #2795, .F. ) ;
#9376 = FACE_OUTER_BOUND ( 'NONE', #3947, .T. ) ;
#9377 = LINE ( 'NONE', #8487, #4576 ) ;
#9378 = VECTOR ( 'NONE', #6701, 1000.000000000000114 ) ;
#9379 = CARTESIAN_POINT ( 'NONE',  ( -10.19839929293507375, 1.081249999044084475, 24.62111388749999108 ) ) ;
#9380 = CARTESIAN_POINT ( 'NONE',  ( 15.60400172474260749, 28.00000000000000000, -12.47307621135338884 ) ) ;
#9381 = DIRECTION ( 'NONE',  ( -0.000000000000000000, -1.000000000000000000, -0.000000000000000000 ) ) ;
#9382 = ADVANCED_FACE ( 'NONE', ( #7322 ), #9092, .T. ) ;
#9383 = DIRECTION ( 'NONE',  ( -0.000000000000000000, -1.000000000000000000, -0.000000000000000000 ) ) ;
#9384 = DIRECTION ( 'NONE',  ( 0.000000000000000000, 0.000000000000000000, -1.000000000000000000 ) ) ;
#9385 = CIRCLE ( 'NONE', #3923, 2.000000000000004441 ) ;
#9386 = AXIS2_PLACEMENT_3D ( 'NONE', #4693, #10582, #10740 ) ;
#9387 = AXIS2_PLACEMENT_3D ( 'NONE', #5244, #6175, #4411 ) ;
#9388 = CARTESIAN_POINT ( 'NONE',  ( 17.40975659021752975, 1.518749999044084698, -17.40975659021752975 ) ) ;
#9389 = CARTESIAN_POINT ( 'NONE',  ( 17.40975659021752975, 3.518749999044084920, -17.40975659021752975 ) ) ;
#9390 = CARTESIAN_POINT ( 'NONE',  ( -5.000000000000000000, 90.00000000000001421, 5.000000000000000000 ) ) ;
#9391 = DIRECTION ( 'NONE',  ( -0.000000000000000000, -1.000000000000000000, -0.000000000000000000 ) ) ;
#9392 = EDGE_LOOP ( 'NONE', ( #3922, #6685, #6157, #5901 ) ) ;
#9393 = CARTESIAN_POINT ( 'NONE',  ( -25.00000000000001066, 3.562500000000000000, 10.35533905932737397 ) ) ;
#9394 = AXIS2_PLACEMENT_3D ( 'NONE', #208, #7360, #7259 ) ;
#9395 = DIRECTION ( 'NONE',  ( -0.000000000000000000, -1.000000000000000000, -0.000000000000000000 ) ) ;
#9396 = AXIS2_PLACEMENT_3D ( 'NONE', #10594, #8101, #695 ) ;
#9397 = CARTESIAN_POINT ( 'NONE',  ( -19.75000000000003197, -0.001000000000001000089, -2.999999999999789946 ) ) ;
#9398 = CARTESIAN_POINT ( 'NONE',  ( 25.00000000000000000, 2.612499998088169129, 0.000000000000000000 ) ) ;
#9399 = CARTESIAN_POINT ( 'NONE',  ( -10.00000000000000000, 90.00000000000001421, 5.000000000000000000 ) ) ;
#9400 = CARTESIAN_POINT ( 'NONE',  ( -17.67766952966368876, 4.375000000000000000, -17.67766952966369232 ) ) ;
#9401 = CIRCLE ( 'NONE', #8699, 6.999999999999997335 ) ;
#9402 = ORIENTED_EDGE ( 'NONE', *, *, #5413, .F. ) ;
#9403 = VECTOR ( 'NONE', #6993, 1000.000000000000000 ) ;
#9404 = PLANE ( 'NONE',  #7055 ) ;
#9405 = CARTESIAN_POINT ( 'NONE',  ( -10.19839929293505776, 2.706249999044084475, -24.62111388750000174 ) ) ;
#9406 = ADVANCED_BREP_SHAPE_REPRESENTATION ( '', ( #10557, #7040 ), #8612 ) ;
#9407 = CARTESIAN_POINT ( 'NONE',  ( -1.500000000000001332, 0.000000000000000000, 0.000000000000000000 ) ) ;
#9408 = CARTESIAN_POINT ( 'NONE',  ( 24.99999999999999289, 4.549999998088169129, 10.35533905932739529 ) ) ;
#9409 = CIRCLE ( 'NONE', #7462, 2.999999999999998668 ) ;
#9410 = CARTESIAN_POINT ( 'NONE',  ( 24.62111388750000174, 4.281249999044084653, -10.19839929293505776 ) ) ;
#9411 = CARTESIAN_POINT ( 'NONE',  ( 82.32050807568876394, 100.2820323027551268, 0.000000000000000000 ) ) ;
#9412 = CIRCLE ( 'NONE', #6771, 4.999999999999997335 ) ;
#9413 = FACE_OUTER_BOUND ( 'NONE', #10669, .T. ) ;
#9414 = FACE_BOUND ( 'NONE', #8945, .T. ) ;
#9415 = FACE_OUTER_BOUND ( 'NONE', #8417, .T. ) ;
#9416 = DIRECTION ( 'NONE',  ( -1.000000000000000000, 0.000000000000000000, 0.000000000000000000 ) ) ;
#9417 = CIRCLE ( 'NONE', #2171, 7.500000000000000888 ) ;
#9418 = CARTESIAN_POINT ( 'NONE',  ( 2.500000000000000444, -6.505213034913026604E-16, -1.154700538379252794 ) ) ;
#9419 = ORIENTED_EDGE ( 'NONE', *, *, #6366, .T. ) ;
#9420 = ORIENTED_EDGE ( 'NONE', *, *, #1514, .T. ) ;
#9421 = EDGE_CURVE ( 'NONE', #375, #9255, #4906, .T. ) ;
#9422 = AXIS2_PLACEMENT_3D ( 'NONE', #3841, #1459, #8089 ) ;
#9423 = ORIENTED_EDGE ( 'NONE', *, *, #4024, .F. ) ;
#9424 = ORIENTED_EDGE ( 'NONE', *, *, #10595, .F. ) ;
#9425 = ORIENTED_EDGE ( 'NONE', *, *, #7200, .F. ) ;
#9426 = DIRECTION ( 'NONE',  ( -0.9449111825230641637, 0.000000000000000000, -0.3273268353539998121 ) ) ;
#9427 = EDGE_CURVE ( 'NONE', #4593, #4029, #8256, .T. ) ;
#9428 = CARTESIAN_POINT ( 'NONE',  ( -1.400000000000001910, 0.000000000000000000, 0.000000000000000000 ) ) ;
#9429 = ORIENTED_EDGE ( 'NONE', *, *, #6294, .T. ) ;
#9430 = FACE_OUTER_BOUND ( 'NONE', #6432, .T. ) ;
#9431 = DIRECTION ( 'NONE',  ( -0.2500000000000041078, -0.8660254037844380415, 0.4330127018922181881 ) ) ;
#9432 = PLANE ( 'NONE',  #5522 ) ;
#9433 = CYLINDRICAL_SURFACE ( 'NONE', #2127, 2.999999999999997335 ) ;
#9434 = LINE ( 'NONE', #7779, #4652 ) ;
#9435 = CARTESIAN_POINT ( 'NONE',  ( 0.000000000000000000, 88.00000000000001421, -30.00000000000000000 ) ) ;
#9436 = ORIENTED_EDGE ( 'NONE', *, *, #5455, .F. ) ;
#9437 = ADVANCED_FACE ( 'NONE', ( #3972 ), #6616, .F. ) ;
#9438 = ORIENTED_EDGE ( 'NONE', *, *, #6063, .F. ) ;
#9439 = EDGE_CURVE ( 'NONE', #9938, #3835, #8883, .T. ) ;
#9440 = PRODUCT_DEFINITION_SHAPE ( 'NONE', 'NONE',  #8315 ) ;
#9441 = CARTESIAN_POINT ( 'NONE',  ( -1.500000000000000444, 88.00000000000001421, -1.500000000000000222 ) ) ;
#9442 = DIRECTION ( 'NONE',  ( 1.000000000000000000, 0.000000000000000000, 3.491481338843133355E-15 ) ) ;
#9443 = CARTESIAN_POINT ( 'NONE',  ( 24.62111388750000174, 1.393749999044084475, 0.000000000000000000 ) ) ;
#9444 = ORIENTED_EDGE ( 'NONE', *, *, #9970, .T. ) ;
#9445 = DIRECTION ( 'NONE',  ( 0.000000000000000000, -1.000000000000000000, 0.000000000000000000 ) ) ;
#9446 = CONTEXT_DEPENDENT_SHAPE_REPRESENTATION ( #6907, #10326 ) ;
#9447 = DIRECTION ( 'NONE',  ( 0.000000000000000000, -1.000000000000000000, 0.000000000000000000 ) ) ;
#9448 = CARTESIAN_POINT ( 'NONE',  ( -20.63749999999999929, 0.000000000000000000, 0.000000000000000000 ) ) ;
#9449 = CARTESIAN_POINT ( 'NONE',  ( -24.62111388750000174, 3.718749999044084653, -3.015216831376932151E-15 ) ) ;
#9450 = ADVANCED_FACE ( 'NONE', ( #8050 ), #4353, .T. ) ;
#9451 = EDGE_CURVE ( 'NONE', #6293, #9491, #8375, .T. ) ;
#9452 = CARTESIAN_POINT ( 'NONE',  ( -10.19839929293507552, 2.081249999044084475, 24.62111388749999463 ) ) ;
#9453 = PLANE ( 'NONE',  #2120 ) ;
#9454 = CARTESIAN_POINT ( 'NONE',  ( -4.522825247065398226E-15, 3.968749999044084209, 24.62111388750000174 ) ) ;
#9455 = CARTESIAN_POINT ( 'NONE',  ( -24.62111388750000174, 1.831249999044084475, -10.19839929293506131 ) ) ;
#9456 = ORIENTED_EDGE ( 'NONE', *, *, #10639, .T. ) ;
#9457 = CARTESIAN_POINT ( 'NONE',  ( -12.69999999999998153, 0.000000000000000000, 2.000000000000004441 ) ) ;
#9458 =( NAMED_UNIT ( * ) PLANE_ANGLE_UNIT ( ) SI_UNIT ( $, .RADIAN. ) );
#9459 = DIRECTION ( 'NONE',  ( -0.000000000000000000, 1.000000000000000000, 0.000000000000000000 ) ) ;
#9460 = CARTESIAN_POINT ( 'NONE',  ( -10.19839929293505776, 0.5312499990440845421, -24.62111388750000174 ) ) ;
#9461 = CARTESIAN_POINT ( 'NONE',  ( 0.000000000000000000, 10.00000000000000355, 0.000000000000000000 ) ) ;
#9462 = CARTESIAN_POINT ( 'NONE',  ( -10.35533905932739174, 3.687500000000000444, 24.99999999999999289 ) ) ;
#9463 = ORIENTED_EDGE ( 'NONE', *, *, #10430, .F. ) ;
#9464 = VERTEX_POINT ( 'NONE', #27 ) ;
#9465 = ORIENTED_EDGE ( 'NONE', *, *, #4841, .F. ) ;
#9466 = ADVANCED_FACE ( 'NONE', ( #6840 ), #5129, .F. ) ;
#9467 = DIRECTION ( 'NONE',  ( 0.000000000000000000, 0.000000000000000000, 1.000000000000000000 ) ) ;
#9468 = CARTESIAN_POINT ( 'NONE',  ( -24.62111388750000174, 2.893749999044084475, -3.015216831376932151E-15 ) ) ;
#9469 = CARTESIAN_POINT ( 'NONE',  ( 82.32050807568876394, 92.28203230275514102, -5.000000000000000000 ) ) ;
#9470 = CARTESIAN_POINT ( 'NONE',  ( 10.35533905932738286, 2.424999998088169129, 24.99999999999999645 ) ) ;
#9471 = CARTESIAN_POINT ( 'NONE',  ( 17.40975659021752620, 4.093749999044084653, 17.40975659021753330 ) ) ;
#9472 = ORIENTED_EDGE ( 'NONE', *, *, #8149, .F. ) ;
#9473 = LINE ( 'NONE', #9529, #3291 ) ;
#9474 = CARTESIAN_POINT ( 'NONE',  ( -6.062177826491031318, 20.00000000000000355, -3.500000000000064393 ) ) ;
#9475 = DIRECTION ( 'NONE',  ( -0.5000000000000039968, 0.000000000000000000, 0.8660254037844363761 ) ) ;
#9476 = DIRECTION ( 'NONE',  ( 0.000000000000000000, -1.000000000000000000, 0.000000000000000000 ) ) ;
#9477 = CARTESIAN_POINT ( 'NONE',  ( 0.000000000000000000, 85.00000000000000000, 0.000000000000000000 ) ) ;
#9478 = ORIENTED_EDGE ( 'NONE', *, *, #5325, .T. ) ;
#9479 = EDGE_LOOP ( 'NONE', ( #333, #6295 ) ) ;
#9480 = ORIENTED_EDGE ( 'NONE', *, *, #2523, .T. ) ;
#9481 = VERTEX_POINT ( 'NONE', #4135 ) ;
#9482 = LINE ( 'NONE', #1154, #4899 ) ;
#9483 = STYLED_ITEM ( 'NONE', ( #1548 ), #10206 ) ;
#9484 = LINE ( 'NONE', #7712, #2333 ) ;
#9485 = CARTESIAN_POINT ( 'NONE',  ( 15.75000000000000000, -0.001000000000001000089, -5.821397334365942453E-14 ) ) ;
#9486 = DIRECTION ( 'NONE',  ( 0.000000000000000000, 1.000000000000000000, 0.000000000000000000 ) ) ;
#9487 = PLANE ( 'NONE',  #9752 ) ;
#9488 = DIRECTION ( 'NONE',  ( 0.000000000000000000, 1.000000000000000000, 0.000000000000000000 ) ) ;
#9489 = CARTESIAN_POINT ( 'NONE',  ( 0.000000000000000000, 1.734723475976807094E-16, 6.250000000000007105 ) ) ;
#9490 = CARTESIAN_POINT ( 'NONE',  ( -17.40975659021752975, 4.768749999044084475, -17.40975659021752975 ) ) ;
#9491 = VERTEX_POINT ( 'NONE', #3328 ) ;
#9492 = AXIS2_PLACEMENT_3D ( 'NONE', #5957, #4244, #5080 ) ;
#9493 = VERTEX_POINT ( 'NONE', #8483 ) ;
#9494 = CLOSED_SHELL ( 'NONE', ( #5519, #1588, #3640, #3402, #4867, #2018, #9199, #5071, #2521, #7672, #7196, #3416, #9382 ) ) ;
#9495 = CARTESIAN_POINT ( 'NONE',  ( 10.35533905932738286, 2.812500000000000000, 24.99999999999999645 ) ) ;
#9496 = PLANE ( 'NONE',  #328 ) ;
#9497 = ADVANCED_FACE ( 'NONE', ( #1694 ), #3511, .F. ) ;
#9498 = CARTESIAN_POINT ( 'NONE',  ( -24.62111388750000174, 3.831249999044084920, -10.19839929293506131 ) ) ;
#9499 = ORIENTED_EDGE ( 'NONE', *, *, #6885, .T. ) ;
#9500 = EDGE_CURVE ( 'NONE', #2327, #2786, #5951, .T. ) ;
#9501 = CARTESIAN_POINT ( 'NONE',  ( 7.347880794884120722E-16, 88.00000000000001421, -6.000000000000000888 ) ) ;
#9502 = LINE ( 'NONE', #9658, #2885 ) ;
#9503 = AXIS2_PLACEMENT_3D ( 'NONE', #1351, #4732, #8087 ) ;
#9504 = CARTESIAN_POINT ( 'NONE',  ( 3.924072712834419718, 10.00000000000000355, 5.796693311223933165 ) ) ;
#9505 = CARTESIAN_POINT ( 'NONE',  ( -10.19839929293505776, 3.531249999044084653, -24.62111388750000174 ) ) ;
#9506 = AXIS2_PLACEMENT_3D ( 'NONE', #4523, #7878, #1085 ) ;
#9507 = EDGE_CURVE ( 'NONE', #10609, #5553, #5026, .T. ) ;
#9508 = CARTESIAN_POINT ( 'NONE',  ( 17.40975659021752620, 5.268749999044085364, 17.40975659021753330 ) ) ;
#9509 = CARTESIAN_POINT ( 'NONE',  ( 15.75000000000001421, -0.001000000000001000089, 2.999999999999942268 ) ) ;
#9510 = AXIS2_PLACEMENT_3D ( 'NONE', #5683, #4864, #3453 ) ;
#9511 = CARTESIAN_POINT ( 'NONE',  ( -24.62111388750000174, 4.718749999044084653, -3.015216831376932151E-15 ) ) ;
#9512 = DIRECTION ( 'NONE',  ( 0.000000000000000000, 1.000000000000000000, 0.000000000000000000 ) ) ;
#9513 = ORIENTED_EDGE ( 'NONE', *, *, #10521, .F. ) ;
#9514 = EDGE_CURVE ( 'NONE', #5242, #8063, #10626, .T. ) ;
#9515 = DIRECTION ( 'NONE',  ( 0.000000000000000000, 1.000000000000000000, 0.000000000000000000 ) ) ;
#9516 = CARTESIAN_POINT ( 'NONE',  ( -25.00000000000000000, 2.437500000000000444, -10.35533905932738108 ) ) ;
#9517 = FACE_BOUND ( 'NONE', #5757, .T. ) ;
#9518 = DIRECTION ( 'NONE',  ( -0.000000000000000000, -1.000000000000000000, -0.000000000000000000 ) ) ;
#9519 = EDGE_CURVE ( 'NONE', #5115, #2663, #4351, .T. ) ;
#9520 = EDGE_LOOP ( 'NONE', ( #4210, #3040, #7095, #4755, #6400 ) ) ;
#9521 = VERTEX_POINT ( 'NONE', #10085 ) ;
#9522 = CARTESIAN_POINT ( 'NONE',  ( -4.522825247065398226E-15, 2.143749999044084920, 24.62111388750000174 ) ) ;
#9523 = ORIENTED_EDGE ( 'NONE', *, *, #9451, .F. ) ;
#9524 = DIRECTION ( 'NONE',  ( 0.000000000000000000, -1.000000000000000000, 0.000000000000000000 ) ) ;
#9525 = CARTESIAN_POINT ( 'NONE',  ( 24.62111388750000174, 0.2187499990440845699, 0.000000000000000000 ) ) ;
#9526 = CARTESIAN_POINT ( 'NONE',  ( -25.00000000000000000, 2.112499998088169129, -3.061616997868383043E-15 ) ) ;
#9527 = CARTESIAN_POINT ( 'NONE',  ( 24.62111388750000174, 5.218749999044084653, 0.000000000000000000 ) ) ;
#9528 = CYLINDRICAL_SURFACE ( 'NONE', #2085, 25.00000000000000000 ) ;
#9529 = CARTESIAN_POINT ( 'NONE',  ( -10.00000000000000000, 93.00000000000001421, 0.000000000000000000 ) ) ;
#9530 = CARTESIAN_POINT ( 'NONE',  ( 20.00000000000000000, 20.00000000000000355, 0.000000000000000000 ) ) ;
#9531 = DIRECTION ( 'NONE',  ( 1.000000000000000000, 0.000000000000000000, 0.000000000000000000 ) ) ;
#9532 = DIRECTION ( 'NONE',  ( 0.000000000000000000, 0.000000000000000000, -1.000000000000000000 ) ) ;
#9533 = CIRCLE ( 'NONE', #4765, 6.750000000000007994 ) ;
#9534 = CARTESIAN_POINT ( 'NONE',  ( -25.00000000000001421, 1.562500000000000000, 10.35533905932737397 ) ) ;
#9535 = LINE ( 'NONE', #6229, #9747 ) ;
#9536 = ORIENTED_EDGE ( 'NONE', *, *, #9107, .F. ) ;
#9537 = ORIENTED_EDGE ( 'NONE', *, *, #2267, .F. ) ;
#9538 = FACE_OUTER_BOUND ( 'NONE', #3401, .T. ) ;
#9539 = AXIS2_PLACEMENT_3D ( 'NONE', #10888, #780, #9990 ) ;
#9540 = FACE_OUTER_BOUND ( 'NONE', #6333, .T. ) ;
#9541 = VERTEX_POINT ( 'NONE', #5900 ) ;
#9542 = DIRECTION ( 'NONE',  ( -0.000000000000000000, -1.000000000000000000, -0.000000000000000000 ) ) ;
#9543 = PLANE ( 'NONE',  #8867 ) ;
#9544 = LINE ( 'NONE', #8717, #762 ) ;
#9545 = CARTESIAN_POINT ( 'NONE',  ( -11.26313972081434223, 10.00000000000000355, -6.348076211353453679 ) ) ;
#9546 = FACE_OUTER_BOUND ( 'NONE', #7800, .T. ) ;
#9547 = CARTESIAN_POINT ( 'NONE',  ( 24.62111388750000174, 4.456249999044084475, -10.19839929293505776 ) ) ;
#9548 = AXIS2_PLACEMENT_3D ( 'NONE', #6055, #3669, #9416 ) ;
#9549 = CIRCLE ( 'NONE', #10943, 6.000000000000000888 ) ;
#9550 = VERTEX_POINT ( 'NONE', #9249 ) ;
#9551 = EDGE_LOOP ( 'NONE', ( #7108, #1556, #1444 ) ) ;
#9552 = EDGE_LOOP ( 'NONE', ( #10798, #9825, #6816, #1428 ) ) ;
#9553 = DIRECTION ( 'NONE',  ( -0.000000000000000000, -1.000000000000000000, -0.000000000000000000 ) ) ;
#9554 = ADVANCED_BREP_SHAPE_REPRESENTATION ( '', ( #3457, #7040 ), #6672 ) ;
#9555 = CARTESIAN_POINT ( 'NONE',  ( -4.522825247065398226E-15, 2.143749999044084920, 24.62111388750000174 ) ) ;
#9556 = LINE ( 'NONE', #9657, #10046 ) ;
#9557 = DIRECTION ( 'NONE',  ( 7.228014483236695816E-17, 0.000000000000000000, -1.000000000000000000 ) ) ;
#9558 = DIRECTION ( 'NONE',  ( -1.000000000000000000, 0.000000000000000000, -0.000000000000000000 ) ) ;
#9559 = ORIENTED_EDGE ( 'NONE', *, *, #1452, .T. ) ;
#9560 = EDGE_CURVE ( 'NONE', #4627, #7939, #746, .T. ) ;
#9561 = VECTOR ( 'NONE', #559, 1000.000000000000000 ) ;
#9562 = CARTESIAN_POINT ( 'NONE',  ( 25.00000000000000000, 2.062500000000000000, -10.35533905932737753 ) ) ;
#9563 = CARTESIAN_POINT ( 'NONE',  ( -25.00000000000000000, 0.5000000000000000000, -3.061616997868383043E-15 ) ) ;
#9564 = LINE ( 'NONE', #1279, #7969 ) ;
#9565 =( NAMED_UNIT ( * ) PLANE_ANGLE_UNIT ( ) SI_UNIT ( $, .RADIAN. ) );
#9566 = EDGE_CURVE ( 'NONE', #10165, #4640, #4817, .T. ) ;
#9567 = DIRECTION ( 'NONE',  ( 0.000000000000000000, 0.000000000000000000, 1.000000000000000000 ) ) ;
#9568 = CARTESIAN_POINT ( 'NONE',  ( -10.19839929293505776, 1.531249999044084653, -24.62111388750000174 ) ) ;
#9569 = CARTESIAN_POINT ( 'NONE',  ( 3.957930336368489021E-15, -0.001000000000001000089, 19.75000000000000000 ) ) ;
#9570 = VECTOR ( 'NONE', #5980, 1000.000000000000000 ) ;
#9571 = ORIENTED_EDGE ( 'NONE', *, *, #6271, .T. ) ;
#9572 = ORIENTED_EDGE ( 'NONE', *, *, #2029, .F. ) ;
#9573 = ADVANCED_FACE ( 'NONE', ( #9651 ), #315, .F. ) ;
#9574 = CIRCLE ( 'NONE', #4812, 12.77350269189627063 ) ;
#9575 = ORIENTED_EDGE ( 'NONE', *, *, #8713, .T. ) ;
#9576 = APPLICATION_CONTEXT ( 'automotive_design' ) ;
#9577 = DIRECTION ( 'NONE',  ( 0.000000000000000000, -2.775557561562888270E-17, -1.000000000000000000 ) ) ;
#9578 = CARTESIAN_POINT ( 'NONE',  ( 17.40975659021752975, 4.343749999044084653, -17.40975659021752975 ) ) ;
#9579 = VECTOR ( 'NONE', #8160, 1000.000000000000000 ) ;
#9580 = CARTESIAN_POINT ( 'NONE',  ( 10.19839929293505953, 3.581249999044085364, -24.62111388750000174 ) ) ;
#9581 = CARTESIAN_POINT ( 'NONE',  ( -17.67766952966368876, 3.987499998088168685, -17.67766952966369232 ) ) ;
#9582 = CARTESIAN_POINT ( 'NONE',  ( 1.530808498934191521E-15, 3.250000000000000444, -25.00000000000000000 ) ) ;
#9583 = EDGE_CURVE ( 'NONE', #5968, #3303, #9434, .T. ) ;
#9584 = DIRECTION ( 'NONE',  ( 0.000000000000000000, 0.000000000000000000, 1.000000000000000000 ) ) ;
#9585 = CIRCLE ( 'NONE', #1118, 2.999999999999997335 ) ;
#9586 = DIRECTION ( 'NONE',  ( 0.000000000000000000, -0.000000000000000000, -1.000000000000000000 ) ) ;
#9587 = CARTESIAN_POINT ( 'NONE',  ( -4.592425496802574367E-15, 2.750000000000000000, 25.00000000000000000 ) ) ;
#9588 = VECTOR ( 'NONE', #7176, 1000.000000000000000 ) ;
#9589 = LINE ( 'NONE', #10356, #4433 ) ;
#9590 = DIRECTION ( 'NONE',  ( -0.000000000000000000, -1.000000000000000000, -0.000000000000000000 ) ) ;
#9591 = VECTOR ( 'NONE', #7881, 1000.000000000000227 ) ;
#9592 = VERTEX_POINT ( 'NONE', #4417 ) ;
#9593 = VERTEX_POINT ( 'NONE', #3686 ) ;
#9594 = AXIS2_PLACEMENT_3D ( 'NONE', #60, #114, #7567 ) ;
#9595 = DIRECTION ( 'NONE',  ( 0.000000000000000000, 0.000000000000000000, -1.000000000000000000 ) ) ;
#9596 = AXIS2_PLACEMENT_3D ( 'NONE', #7080, #483, #2798 ) ;
#9597 = ADVANCED_FACE ( 'NONE', ( #9546 ), #426, .T. ) ;
#9598 = VECTOR ( 'NONE', #944, 1000.000000000000000 ) ;
#9599 = CARTESIAN_POINT ( 'NONE',  ( -19.74999999999996803, 25.00000000000000000, 3.000000000000206057 ) ) ;
#9600 = DIRECTION ( 'NONE',  ( -1.000000000000000000, 0.000000000000000000, 0.000000000000000000 ) ) ;
#9601 = CYLINDRICAL_SURFACE ( 'NONE', #2679, 2.999999999999999112 ) ;
#9602 = DIRECTION ( 'NONE',  ( 0.000000000000000000, 1.000000000000000000, 0.000000000000000000 ) ) ;
#9603 = CARTESIAN_POINT ( 'NONE',  ( 67.97877056362573001, 94.28203230275514102, 5.000000000000000000 ) ) ;
#9604 = FACE_OUTER_BOUND ( 'NONE', #1196, .T. ) ;
#9605 = ORIENTED_EDGE ( 'NONE', *, *, #4030, .T. ) ;
#9606 = AXIS2_PLACEMENT_3D ( 'NONE', #1572, #3326, #10083 ) ;
#9607 = ORIENTED_EDGE ( 'NONE', *, *, #6543, .T. ) ;
#9608 = LINE ( 'NONE', #5559, #6153 ) ;
#9609 = CARTESIAN_POINT ( 'NONE',  ( -4.522825247065398226E-15, 3.143749999044084475, 24.62111388750000174 ) ) ;
#9610 = CARTESIAN_POINT ( 'NONE',  ( 12.47307621135322186, -0.001000000000001000089, -15.60400172474273717 ) ) ;
#9611 = CARTESIAN_POINT ( 'NONE',  ( 0.000000000000000000, 20.00000000000000355, -2.149999999999999911 ) ) ;
#9612 = CARTESIAN_POINT ( 'NONE',  ( 0.000000000000000000, 0.000000000000000000, -5.000000000000000000 ) ) ;
#9613 = LINE ( 'NONE', #5462, #7109 ) ;
#9614 = ORIENTED_EDGE ( 'NONE', *, *, #8200, .T. ) ;
#9615 = ORIENTED_EDGE ( 'NONE', *, *, #7014, .T. ) ;
#9616 = CARTESIAN_POINT ( 'NONE',  ( -17.40975659021752975, 4.768749999044084475, -17.40975659021752975 ) ) ;
#9617 = PLANE ( 'NONE',  #7246 ) ;
#9618 = PLANE ( 'NONE',  #320 ) ;
#9619 = DIRECTION ( 'NONE',  ( 0.000000000000000000, -1.000000000000000000, 0.000000000000000000 ) ) ;
#9620 = EDGE_LOOP ( 'NONE', ( #4972, #10246, #5420, #5031 ) ) ;
#9621 = DIRECTION ( 'NONE',  ( 0.000000000000000000, -2.775557561562888270E-17, -1.000000000000000000 ) ) ;
#9622 = DIRECTION ( 'NONE',  ( 0.000000000000000000, 1.000000000000000000, 0.000000000000000000 ) ) ;
#9623 = CARTESIAN_POINT ( 'NONE',  ( -24.62111388750000884, 2.781249999044085097, 10.19839929293505421 ) ) ;
#9624 = EDGE_CURVE ( 'NONE', #5481, #2342, #10804, .T. ) ;
#9625 = CARTESIAN_POINT ( 'NONE',  ( 17.67766952966369232, 4.125000000000000000, -17.67766952966369232 ) ) ;
#9626 = ORIENTED_EDGE ( 'NONE', *, *, #8949, .T. ) ;
#9627 = ORIENTED_EDGE ( 'NONE', *, *, #7336, .F. ) ;
#9628 = EDGE_CURVE ( 'NONE', #7410, #9311, #6759, .T. ) ;
#9629 = CARTESIAN_POINT ( 'NONE',  ( 0.000000000000000000, 20.00000000000000355, 6.999999999999997335 ) ) ;
#9630 = CARTESIAN_POINT ( 'NONE',  ( -17.40975659021753330, 2.843749999044085097, 17.40975659021752975 ) ) ;
#9631 = CARTESIAN_POINT ( 'NONE',  ( -10.19839929293507552, 5.081249999044084475, 24.62111388749999463 ) ) ;
#9632 = CARTESIAN_POINT ( 'NONE',  ( -25.00000000000000000, 3.500000000000000000, -3.061616997868383043E-15 ) ) ;
#9633 = ADVANCED_FACE ( 'NONE', ( #9604 ), #5250, .F. ) ;
#9634 = EDGE_CURVE ( 'NONE', #10381, #4561, #8318, .T. ) ;
#9635 = CARTESIAN_POINT ( 'NONE',  ( -11.12916512459892893, 10.00000000000000355, 6.580127018922093285 ) ) ;
#9636 = LINE ( 'NONE', #10566, #10418 ) ;
#9637 = ADVANCED_FACE ( 'NONE', ( #1102 ), #7118, .F. ) ;
#9638 = CARTESIAN_POINT ( 'NONE',  ( 68.37372805638788975, 97.28203230275514102, 5.000000000000000000 ) ) ;
#9639 = LINE ( 'NONE', #6226, #539 ) ;
#9640 = CARTESIAN_POINT ( 'NONE',  ( 17.67766952966368521, 1.875000000000000000, 17.67766952966369232 ) ) ;
#9641 = ORIENTED_EDGE ( 'NONE', *, *, #3176, .T. ) ;
#9642 = ORIENTED_EDGE ( 'NONE', *, *, #5885, .F. ) ;
#9643 = ORIENTED_EDGE ( 'NONE', *, *, #3435, .T. ) ;
#9644 = ADVANCED_FACE ( 'NONE', ( #7840 ), #4479, .T. ) ;
#9645 = LINE ( 'NONE', #6440, #6317 ) ;
#9646 = CYLINDRICAL_SURFACE ( 'NONE', #2505, 2.999999999999999112 ) ;
#9647 = ADVANCED_FACE ( 'NONE', ( #6128 ), #6075, .T. ) ;
#9648 = DIRECTION ( 'NONE',  ( 0.000000000000000000, -1.000000000000000000, 0.000000000000000000 ) ) ;
#9649 = DIRECTION ( 'NONE',  ( -0.000000000000000000, -1.000000000000000000, -0.000000000000000000 ) ) ;
#9650 = CARTESIAN_POINT ( 'NONE',  ( 0.5000000000000000000, 10.00000000000000355, 6.982120021884467675 ) ) ;
#9651 = FACE_OUTER_BOUND ( 'NONE', #5253, .T. ) ;
#9652 = EDGE_LOOP ( 'NONE', ( #5967, #10041, #4779, #9033 ) ) ;
#9653 = ADVANCED_FACE ( 'NONE', ( #1044 ), #3571, .F. ) ;
#9654 = ORIENTED_EDGE ( 'NONE', *, *, #10607, .T. ) ;
#9655 = CARTESIAN_POINT ( 'NONE',  ( 82.32050807568876394, 92.28203230275514102, 4.000000000000006217 ) ) ;
#9656 =( BOUNDED_CURVE ( )  B_SPLINE_CURVE ( 2, ( #8926, #5569, #4018, #9858, #3969 ),
 .UNSPECIFIED., .F., .F. ) 
 B_SPLINE_CURVE_WITH_KNOTS ( ( 3, 2, 3 ),
 ( 0.000000000000000000, 0.02500000000000000486, 0.05000000000000000971 ),
 .UNSPECIFIED. ) 
 CURVE ( )  GEOMETRIC_REPRESENTATION_ITEM ( )  RATIONAL_B_SPLINE_CURVE ( ( 1.000000000000000000, 0.9238795325112867385, 1.000000000000000000, 0.9238795325112867385, 1.000000000000000000 ) ) 
 REPRESENTATION_ITEM ( '' )  );
#9657 = CARTESIAN_POINT ( 'NONE',  ( 0.5000000000000000000, 10.00000000000000355, 6.999999999999997335 ) ) ;
#9658 = CARTESIAN_POINT ( 'NONE',  ( 0.000000000000000000, 5.000000000000000000, -25.00000000000000000 ) ) ;
#9659 = CARTESIAN_POINT ( 'NONE',  ( -10.47307621135315792, 25.00000000000000000, 12.13990010960504762 ) ) ;
#9660 = CARTESIAN_POINT ( 'NONE',  ( 0.000000000000000000, 10.00000000000000355, 0.000000000000000000 ) ) ;
#9661 = EDGE_CURVE ( 'NONE', #6472, #4266, #1255, .T. ) ;
#9662 = CIRCLE ( 'NONE', #6664, 2.999999999999996891 ) ;
#9663 = VERTEX_POINT ( 'NONE', #7992 ) ;
#9664 = VERTEX_POINT ( 'NONE', #6180 ) ;
#9665 = CYLINDRICAL_SURFACE ( 'NONE', #3162, 6.999999999999997335 ) ;
#9666 = AXIS2_PLACEMENT_3D ( 'NONE', #2803, #2144, #7181 ) ;
#9667 = CARTESIAN_POINT ( 'NONE',  ( -23.00215391598666059, 5.000000000000000000, 9.113568881329346283 ) ) ;
#9668 = CARTESIAN_POINT ( 'NONE',  ( -24.62111388750000174, 0.8312499990440843645, -10.19839929293506131 ) ) ;
#9669 = ORIENTED_EDGE ( 'NONE', *, *, #4549, .T. ) ;
#9670 = DIRECTION ( 'NONE',  ( -0.000000000000000000, 1.000000000000000000, -0.000000000000000000 ) ) ;
#9671 =( LENGTH_UNIT ( ) NAMED_UNIT ( * ) SI_UNIT ( .MILLI., .METRE. ) );
#9672 = CARTESIAN_POINT ( 'NONE',  ( 0.000000000000000000, -58.00000000000000000, 0.000000000000000000 ) ) ;
#9673 = ORIENTED_EDGE ( 'NONE', *, *, #6458, .T. ) ;
#9674 = VECTOR ( 'NONE', #7103, 1000.000000000000114 ) ;
#9675 = CARTESIAN_POINT ( 'NONE',  ( 10.19839929293505953, 1.406249999044084209, -24.62111388750000174 ) ) ;
#9676 = DIRECTION ( 'NONE',  ( -0.000000000000000000, 1.000000000000000000, -0.000000000000000000 ) ) ;
#9677 = ORIENTED_EDGE ( 'NONE', *, *, #10167, .T. ) ;
#9678 = ORIENTED_EDGE ( 'NONE', *, *, #931, .T. ) ;
#9679 = STYLED_ITEM ( 'NONE', ( #7528 ), #10772 ) ;
#9680 = VECTOR ( 'NONE', #1644, 1000.000000000000000 ) ;
#9681 = CARTESIAN_POINT ( 'NONE',  ( 6.348076211353333775, 10.00000000000000355, -11.26313972081440618 ) ) ;
#9682 = CARTESIAN_POINT ( 'NONE',  ( -10.19839929293505776, 1.531249999044084653, -24.62111388750000174 ) ) ;
#9683 = CARTESIAN_POINT ( 'NONE',  ( -24.62111388750000884, 3.956249999044084920, 10.19839929293505421 ) ) ;
#9684 = CARTESIAN_POINT ( 'NONE',  ( 10.35533905932737930, 2.187500000000000444, -25.00000000000000000 ) ) ;
#9685 = LINE ( 'NONE', #3829, #2253 ) ;
#9686 = CARTESIAN_POINT ( 'NONE',  ( 3.499999999999996447, 20.00000000000000355, -6.062177826491068622 ) ) ;
#9687 = CARTESIAN_POINT ( 'NONE',  ( 0.000000000000000000, 10.00000000000000355, 0.000000000000000000 ) ) ;
#9688 = ORIENTED_EDGE ( 'NONE', *, *, #10452, .F. ) ;
#9689 = EDGE_CURVE ( 'NONE', #6119, #1843, #6755, .T. ) ;
#9690 = LINE ( 'NONE', #5406, #6665 ) ;
#9691 = CARTESIAN_POINT ( 'NONE',  ( 0.000000000000000000, -55.00000000000000000, 0.000000000000000000 ) ) ;
#9692 = AXIS2_PLACEMENT_3D ( 'NONE', #8325, #10881, #3342 ) ;
#9693 = DIRECTION ( 'NONE',  ( 0.000000000000000000, -2.775557561562888270E-17, -1.000000000000000000 ) ) ;
#9694 = EDGE_CURVE ( 'NONE', #8014, #9966, #3844, .T. ) ;
#9695 = LINE ( 'NONE', #473, #9913 ) ;
#9696 = DIRECTION ( 'NONE',  ( -0.000000000000000000, 1.000000000000000000, -0.000000000000000000 ) ) ;
#9697 = CYLINDRICAL_SURFACE ( 'NONE', #6068, 2.999999999999999112 ) ;
#9698 = VERTEX_POINT ( 'NONE', #578 ) ;
#9699 = ORIENTED_EDGE ( 'NONE', *, *, #9689, .F. ) ;
#9700 = CIRCLE ( 'NONE', #9368, 7.500000000000007994 ) ;
#9701 = CIRCLE ( 'NONE', #2454, 6.999999999999997335 ) ;
#9702 = EDGE_CURVE ( 'NONE', #5192, #7897, #8148, .T. ) ;
#9703 = VERTEX_POINT ( 'NONE', #2231 ) ;
#9704 = CARTESIAN_POINT ( 'NONE',  ( 25.10306914047445659, 102.1838626489802380, 5.000000000000000000 ) ) ;
#9705 = CARTESIAN_POINT ( 'NONE',  ( 2.500000000000000444, -4.336808689942017736E-16, 1.154700538379254571 ) ) ;
#9706 = EDGE_CURVE ( 'NONE', #4100, #634, #4286, .T. ) ;
#9707 = DIRECTION ( 'NONE',  ( 0.4999999999999951705, 0.000000000000000000, -0.8660254037844413721 ) ) ;
#9708 = CIRCLE ( 'NONE', #7771, 25.00000000000000000 ) ;
#9709 = CIRCLE ( 'NONE', #6720, 2.999999999999996891 ) ;
#9710 = CARTESIAN_POINT ( 'NONE',  ( -15.60400172474278158, 25.00000000000000000, -12.47307621135316680 ) ) ;
#9711 = FACE_OUTER_BOUND ( 'NONE', #3273, .T. ) ;
#9712 =( REPRESENTATION_RELATIONSHIP ('NONE','NONE', #1269, #2382 ) REPRESENTATION_RELATIONSHIP_WITH_TRANSFORMATION ( #5961 )SHAPE_REPRESENTATION_RELATIONSHIP( ) );
#9713 = ORIENTED_EDGE ( 'NONE', *, *, #10657, .T. ) ;
#9714 = AXIS2_PLACEMENT_3D ( 'NONE', #3685, #7893, #1868 ) ;
#9715 = VECTOR ( 'NONE', #5630, 1000.000000000000000 ) ;
#9716 =( BOUNDED_SURFACE ( )  B_SPLINE_SURFACE ( 1, 2, ( 
 ( #5923, #6865, #6986, #6151, #3419, #1951, #4512, #1778, #6101, #8565, #5328, #290, #8682, #6810, #7866, #2581, #5979, #1716, #5096, #9329, #5157, #8506, #7687, #960, #116, #3476, #2704, #10224, #3536, #2641, #4382, #6037, #9398, #7745, #4927, #9940, #3081, #5746, #6474, #1494, #7294, #552, #8180, #9828, #10612, #4823, #4766, #3181, #9064, #10833, #3936, #1542, #8337, #718, #6524, #8275, #5646, #6429, #9779, #3028, #4097, #6580, #10775, #8121, #4875, #2211, #9004, #10670, #1430, #9163, #2262, #8222, #609, #2417, #10716, #7342, #7454, #3232, #1597, #2371, #3990 ),
 ( #3130, #9880, #5591, #6631, #2315, #9989, #779, #1381, #5699, #662, #5800, #4983, #8951, #4149, #4042, #7396, #8615, #5149, #8498, #951, #10213, #52, #1003, #8439, #6029, #1706, #887, #9452, #4198, #4317, #4256, #10944, #4371, #9264, #3349, #8556, #3411, #6803, #3466, #3527, #6746, #7677, #6921, #10161, #107, #6857, #6692, #2632, #2524, #2574, #9389, #10279, #830, #5970, #1832, #5858, #5915, #5213, #6092, #1060, #1884, #9321, #7509, #10887, #3289, #10049, #1772, #2470, #9216, #1659, #9616, #7959, #1174, #3759, #3702, #10443, #2904, #282, #9508, #7136, #8833 ) ),
 .UNSPECIFIED., .F., .F., .F. ) 
 B_SPLINE_SURFACE_WITH_KNOTS ( ( 2, 2 ),
 ( 3, 2, 2, 2, 2, 2, 2, 2, 2, 2, 2, 2, 2, 2, 2, 2, 2, 2, 2, 2, 2, 2, 2, 2, 2, 2, 2, 2, 2, 2, 2, 2, 2, 2, 2, 2, 2, 2, 2, 2, 3 ),
 ( 0.000000000000000000, 1.000000000000000000 ),
 ( 0.000000000000000000, 0.02500000000000000139, 0.05000000000000000278, 0.07499999999999999722, 0.1000000000000000056, 0.1250000000000000000, 0.1499999999999999944, 0.1749999999999999889, 0.2000000000000000111, 0.2250000000000000056, 0.2500000000000000000, 0.2750000000000000222, 0.2999999999999999889, 0.3250000000000000111, 0.3499999999999999778, 0.3750000000000000000, 0.4000000000000000222, 0.4249999999999999889, 0.4500000000000000111, 0.4749999999999999778, 0.5000000000000000000, 0.5250000000000000222, 0.5500000000000000444, 0.5749999999999999556, 0.5999999999999999778, 0.6250000000000000000, 0.6500000000000000222, 0.6750000000000000444, 0.6999999999999999556, 0.7249999999999999778, 0.7500000000000000000, 0.7750000000000000222, 0.8000000000000000444, 0.8249999999999999556, 0.8499999999999999778, 0.8750000000000000000, 0.9000000000000000222, 0.9250000000000000444, 0.9499999999999999556, 0.9749999999999999778, 1.000000000000000000 ),
 .UNSPECIFIED. ) 
 GEOMETRIC_REPRESENTATION_ITEM ( )  RATIONAL_B_SPLINE_SURFACE ( (
 ( 1.000000000000000000, 0.9238795325112867385, 1.000000000000000000, 0.9238795325112867385, 1.000000000000000000, 0.9238795325112867385, 1.000000000000000000, 0.9238795325112867385, 1.000000000000000000, 0.9238795325112867385, 1.000000000000000000, 0.9238795325112867385, 1.000000000000000000, 0.9238795325112867385, 1.000000000000000000, 0.9238795325112867385, 1.000000000000000000, 0.9238795325112867385, 1.000000000000000000, 0.9238795325112867385, 1.000000000000000000, 0.9238795325112867385, 1.000000000000000000, 0.9238795325112867385, 1.000000000000000000, 0.9238795325112867385, 1.000000000000000000, 0.9238795325112867385, 1.000000000000000000, 0.9238795325112867385, 1.000000000000000000, 0.9238795325112867385, 1.000000000000000000, 0.9238795325112867385, 1.000000000000000000, 0.9238795325112867385, 1.000000000000000000, 0.9238795325112867385, 1.000000000000000000, 0.9238795325112867385, 1.000000000000000000, 0.9238795325112867385, 1.000000000000000000, 0.9238795325112867385, 1.000000000000000000, 0.9238795325112867385, 1.000000000000000000, 0.9238795325112867385, 1.000000000000000000, 0.9238795325112867385, 1.000000000000000000, 0.9238795325112867385, 1.000000000000000000, 0.9238795325112867385, 1.000000000000000000, 0.9238795325112867385, 1.000000000000000000, 0.9238795325112867385, 1.000000000000000000, 0.9238795325112867385, 1.000000000000000000, 0.9238795325112867385, 1.000000000000000000, 0.9238795325112867385, 1.000000000000000000, 0.9238795325112867385, 1.000000000000000000, 0.9238795325112867385, 1.000000000000000000, 0.9238795325112867385, 1.000000000000000000, 0.9238795325112867385, 1.000000000000000000, 0.9238795325112867385, 1.000000000000000000, 0.9238795325112867385, 1.000000000000000000, 0.9238795325112867385, 1.000000000000000000, 0.9238795325112867385, 1.000000000000000000),
 ( 1.000000000000000000, 0.9238795325112867385, 1.000000000000000000, 0.9238795325112867385, 1.000000000000000000, 0.9238795325112867385, 1.000000000000000000, 0.9238795325112867385, 1.000000000000000000, 0.9238795325112867385, 1.000000000000000000, 0.9238795325112867385, 1.000000000000000000, 0.9238795325112867385, 1.000000000000000000, 0.9238795325112867385, 1.000000000000000000, 0.9238795325112867385, 1.000000000000000000, 0.9238795325112867385, 1.000000000000000000, 0.9238795325112867385, 1.000000000000000000, 0.9238795325112867385, 1.000000000000000000, 0.9238795325112867385, 1.000000000000000000, 0.9238795325112867385, 1.000000000000000000, 0.9238795325112867385, 1.000000000000000000, 0.9238795325112867385, 1.000000000000000000, 0.9238795325112867385, 1.000000000000000000, 0.9238795325112867385, 1.000000000000000000, 0.9238795325112867385, 1.000000000000000000, 0.9238795325112867385, 1.000000000000000000, 0.9238795325112867385, 1.000000000000000000, 0.9238795325112867385, 1.000000000000000000, 0.9238795325112867385, 1.000000000000000000, 0.9238795325112867385, 1.000000000000000000, 0.9238795325112867385, 1.000000000000000000, 0.9238795325112867385, 1.000000000000000000, 0.9238795325112867385, 1.000000000000000000, 0.9238795325112867385, 1.000000000000000000, 0.9238795325112867385, 1.000000000000000000, 0.9238795325112867385, 1.000000000000000000, 0.9238795325112867385, 1.000000000000000000, 0.9238795325112867385, 1.000000000000000000, 0.9238795325112867385, 1.000000000000000000, 0.9238795325112867385, 1.000000000000000000, 0.9238795325112867385, 1.000000000000000000, 0.9238795325112867385, 1.000000000000000000, 0.9238795325112867385, 1.000000000000000000, 0.9238795325112867385, 1.000000000000000000, 0.9238795325112867385, 1.000000000000000000, 0.9238795325112867385, 1.000000000000000000) ) ) 
 REPRESENTATION_ITEM ( '' )  SURFACE ( )  );
#9717 = DIRECTION ( 'NONE',  ( -0.000000000000000000, 0.000000000000000000, -1.000000000000000000 ) ) ;
#9718 = CARTESIAN_POINT ( 'NONE',  ( -19.96339341614531193, 5.000000000000000888, -15.08987035441359303 ) ) ;
#9719 = CARTESIAN_POINT ( 'NONE',  ( -24.62111388750000174, 3.831249999044084920, -10.19839929293506131 ) ) ;
#9720 = EDGE_CURVE ( 'NONE', #5566, #824, #7261, .T. ) ;
#9721 = ORIENTED_EDGE ( 'NONE', *, *, #2984, .F. ) ;
#9722 = CARTESIAN_POINT ( 'NONE',  ( 9.184850993605149917E-16, 31.00000000000000000, 7.500000000000000888 ) ) ;
#9723 = CARTESIAN_POINT ( 'NONE',  ( 6.999999999999997335, 20.00000000000000355, 2.444036937190192402E-14 ) ) ;
#9724 = ORIENTED_EDGE ( 'NONE', *, *, #7416, .F. ) ;
#9725 = CARTESIAN_POINT ( 'NONE',  ( 17.40975659021752975, 2.343749999044085097, -17.40975659021752975 ) ) ;
#9726 = CARTESIAN_POINT ( 'NONE',  ( 0.000000000000000000, 82.00000000000000000, 25.00000000000000000 ) ) ;
#9727 = EDGE_LOOP ( 'NONE', ( #1195, #1912, #5161, #214 ) ) ;
#9728 = AXIS2_PLACEMENT_3D ( 'NONE', #2767, #1027, #193 ) ;
#9729 = VERTEX_POINT ( 'NONE', #3099 ) ;
#9730 = CARTESIAN_POINT ( 'NONE',  ( -17.40975659021752975, 1.593749999044084431, -17.40975659021752975 ) ) ;
#9731 = CARTESIAN_POINT ( 'NONE',  ( -24.62111388750000174, 1.893749999044084475, -3.015216831376932151E-15 ) ) ;
#9732 = CARTESIAN_POINT ( 'NONE',  ( 17.67766952966368521, 2.875000000000000000, 17.67766952966369232 ) ) ;
#9733 = AXIS2_PLACEMENT_3D ( 'NONE', #3420, #6931, #8507 ) ;
#9734 = PLANE ( 'NONE',  #7571 ) ;
#9735 = CARTESIAN_POINT ( 'NONE',  ( -9.874999999999777955, -0.001000000000001000089, 17.10400172474279401 ) ) ;
#9736 = CARTESIAN_POINT ( 'NONE',  ( 10.35533905932737930, 1.187500000000000000, -25.00000000000000000 ) ) ;
#9737 = VECTOR ( 'NONE', #6462, 1000.000000000000227 ) ;
#9738 = ORIENTED_EDGE ( 'NONE', *, *, #8094, .F. ) ;
#9739 = EDGE_LOOP ( 'NONE', ( #3262, #4839, #83, #3084 ) ) ;
#9740 = ORIENTED_EDGE ( 'NONE', *, *, #5768, .F. ) ;
#9741 = AXIS2_PLACEMENT_3D ( 'NONE', #370, #2675, #5360 ) ;
#9742 = DIRECTION ( 'NONE',  ( -1.000000000000000000, 0.000000000000000000, 1.047444401652939533E-14 ) ) ;
#9743 = AXIS2_PLACEMENT_3D ( 'NONE', #2553, #3266, #7489 ) ;
#9744 = CARTESIAN_POINT ( 'NONE',  ( 0.000000000000000000, 5.000000000000000000, -22.00000000000000355 ) ) ;
#9745 = CARTESIAN_POINT ( 'NONE',  ( -1.500000000000001332, 0.000000000000000000, 0.000000000000000000 ) ) ;
#9746 = LINE ( 'NONE', #10635, #7795 ) ;
#9747 = VECTOR ( 'NONE', #10309, 1000.000000000000000 ) ;
#9748 = EDGE_CURVE ( 'NONE', #7240, #3964, #5181, .T. ) ;
#9749 = LINE ( 'NONE', #8811, #10768 ) ;
#9750 = AXIS2_PLACEMENT_3D ( 'NONE', #447, #9622, #1949 ) ;
#9751 = VERTEX_POINT ( 'NONE', #2288 ) ;
#9752 = AXIS2_PLACEMENT_3D ( 'NONE', #7011, #7892, #3683 ) ;
#9753 = ADVANCED_FACE ( 'NONE', ( #8920 ), #4791, .T. ) ;
#9754 = VERTEX_POINT ( 'NONE', #2341 ) ;
#9755 = VECTOR ( 'NONE', #5908, 1000.000000000000000 ) ;
#9756 = CARTESIAN_POINT ( 'NONE',  ( 12.19615242270662847, 10.00000000000000355, 0.5000000000000426326 ) ) ;
#9757 = FACE_OUTER_BOUND ( 'NONE', #9791, .T. ) ;
#9758 = LINE ( 'NONE', #10491, #9588 ) ;
#9759 = EDGE_CURVE ( 'NONE', #2, #492, #405, .T. ) ;
#9760 = CARTESIAN_POINT ( 'NONE',  ( -4.592425496802574367E-15, 1.750000000000000000, 25.00000000000000000 ) ) ;
#9761 = EDGE_CURVE ( 'NONE', #883, #10398, #8871, .T. ) ;
#9762 = AXIS2_PLACEMENT_3D ( 'NONE', #1637, #6837, #8310 ) ;
#9763 = VERTEX_POINT ( 'NONE', #2996 ) ;
#9764 = VECTOR ( 'NONE', #7113, 1000.000000000000114 ) ;
#9765 = EDGE_CURVE ( 'NONE', #5101, #1433, #10691, .T. ) ;
#9766 = EDGE_LOOP ( 'NONE', ( #3988, #8438, #9211, #6346, #9677, #1480 ) ) ;
#9767 = DIRECTION ( 'NONE',  ( 0.000000000000000000, -0.8660254037844391517, -0.4999999999999992784 ) ) ;
#9768 = DIRECTION ( 'NONE',  ( 0.000000000000000000, 1.000000000000000000, -0.000000000000000000 ) ) ;
#9769 = VERTEX_POINT ( 'NONE', #9800 ) ;
#9770 = CARTESIAN_POINT ( 'NONE',  ( -20.63749999999999574, -1.935951399190116865E-16, -6.975000000000008527 ) ) ;
#9771 = CARTESIAN_POINT ( 'NONE',  ( 82.32050807568876394, 102.2820323027551410, 0.000000000000000000 ) ) ;
#9772 = CARTESIAN_POINT ( 'NONE',  ( -10.19839929293507375, 2.906249999044085541, 24.62111388749999108 ) ) ;
#9773 = CARTESIAN_POINT ( 'NONE',  ( 25.00000000000000000, -2.710505431213761085E-17, 0.000000000000000000 ) ) ;
#9774 = ORIENTED_EDGE ( 'NONE', *, *, #7323, .F. ) ;
#9775 =( BOUNDED_CURVE ( )  B_SPLINE_CURVE ( 3, ( #6501, #5676, #639, #5731 ),
 .UNSPECIFIED., .F., .F. ) 
 B_SPLINE_CURVE_WITH_KNOTS ( ( 4, 4 ),
 ( 3.927175151554401111, 3.998664601439922084 ),
 .UNSPECIFIED. ) 
 CURVE ( )  GEOMETRIC_REPRESENTATION_ITEM ( )  RATIONAL_B_SPLINE_CURVE ( ( 1.000000000000000000, 0.9995741502243209453, 0.9995741502243209453, 1.000000000000000000 ) ) 
 REPRESENTATION_ITEM ( '' )  );
#9776 = ADVANCED_FACE ( 'NONE', ( #4850 ), #6494, .T. ) ;
#9777 = ORIENTED_EDGE ( 'NONE', *, *, #1938, .F. ) ;
#9778 = EDGE_CURVE ( 'NONE', #1422, #9950, #6395, .T. ) ;
#9779 = CARTESIAN_POINT ( 'NONE',  ( -17.67766952966369232, 4.237499998088169129, 17.67766952966368876 ) ) ;
#9780 = DIRECTION ( 'NONE',  ( 0.000000000000000000, -2.775557561562888270E-17, -1.000000000000000000 ) ) ;
#9781 = CARTESIAN_POINT ( 'NONE',  ( -10.19839929293505776, 2.706249999044084475, -24.62111388750000174 ) ) ;
#9782 = CARTESIAN_POINT ( 'NONE',  ( -10.35533905932739174, 2.687500000000000888, 24.99999999999999289 ) ) ;
#9783 = CARTESIAN_POINT ( 'NONE',  ( 0.000000000000000000, 0.000000000000000000, 0.000000000000000000 ) ) ;
#9784 = CARTESIAN_POINT ( 'NONE',  ( -6.999999999999997335, 20.00000000000000355, -7.332110811570577522E-14 ) ) ;
#9785 = CARTESIAN_POINT ( 'NONE',  ( 5.796693311223893197, 10.00000000000000355, 3.924072712834480559 ) ) ;
#9786 = LINE ( 'NONE', #7978, #4092 ) ;
#9787 = DIRECTION ( 'NONE',  ( -0.4330127018922207971, 0.8660254037844380415, 0.2499999999999995282 ) ) ;
#9788 = EDGE_LOOP ( 'NONE', ( #8785, #10045 ) ) ;
#9789 = EDGE_CURVE ( 'NONE', #5382, #5890, #7896, .T. ) ;
#9790 = ORIENTED_EDGE ( 'NONE', *, *, #1928, .F. ) ;
#9791 = EDGE_LOOP ( 'NONE', ( #7188, #5740, #7573, #5388 ) ) ;
#9792 = ORIENTED_EDGE ( 'NONE', *, *, #10592, .T. ) ;
#9793 = CARTESIAN_POINT ( 'NONE',  ( -10.35533905932738108, 0.6875000000000002220, 24.99999999999999645 ) ) ;
#9794 = CARTESIAN_POINT ( 'NONE',  ( -13.63990010960481492, -0.001000000000001000089, 7.875000000000163425 ) ) ;
#9795 = FILL_AREA_STYLE_COLOUR ( '', #5609 ) ;
#9796 = ORIENTED_EDGE ( 'NONE', *, *, #2219, .T. ) ;
#9797 = CARTESIAN_POINT ( 'NONE',  ( 3.061616997868383043E-15, 25.00000000000000000, 25.00000000000000000 ) ) ;
#9798 = DIRECTION ( 'NONE',  ( 0.000000000000000000, 0.000000000000000000, 1.000000000000000000 ) ) ;
#9799 = CARTESIAN_POINT ( 'NONE',  ( 0.000000000000000000, 25.00000000000000000, 0.000000000000000000 ) ) ;
#9800 = CARTESIAN_POINT ( 'NONE',  ( -1.500000000000000444, 88.00000000000001421, 1.499999999999999778 ) ) ;
#9801 = ORIENTED_EDGE ( 'NONE', *, *, #1075, .F. ) ;
#9802 = ORIENTED_EDGE ( 'NONE', *, *, #6854, .F. ) ;
#9803 = DIRECTION ( 'NONE',  ( 0.000000000000000000, 1.502202555303639631E-16, 1.000000000000000000 ) ) ;
#9804 = FACE_OUTER_BOUND ( 'NONE', #10788, .T. ) ;
#9805 = CARTESIAN_POINT ( 'NONE',  ( 0.000000000000000000, 31.00000000000000000, 0.000000000000000000 ) ) ;
#9806 = CARTESIAN_POINT ( 'NONE',  ( -6.566987298107773263, 19.75000000000000355, -0.5000000000000687228 ) ) ;
#9807 = LINE ( 'NONE', #1416, #935 ) ;
#9808 = ORIENTED_EDGE ( 'NONE', *, *, #7843, .T. ) ;
#9809 = ORIENTED_EDGE ( 'NONE', *, *, #5993, .F. ) ;
#9810 = EDGE_CURVE ( 'NONE', #4041, #9293, #8163, .T. ) ;
#9811 = ADVANCED_FACE ( 'NONE', ( #2941 ), #9697, .F. ) ;
#9812 = CARTESIAN_POINT ( 'NONE',  ( -20.63749999999999574, -2.081668171172168513E-16, -7.500000000000007994 ) ) ;
#9813 = FILL_AREA_STYLE ('',( #6461 ) ) ;
#9814 = LINE ( 'NONE', #491, #10456 ) ;
#9815 = EDGE_LOOP ( 'NONE', ( #2433, #8772, #7550, #1946 ) ) ;
#9816 = FACE_OUTER_BOUND ( 'NONE', #4713, .T. ) ;
#9817 = PRODUCT_CONTEXT ( 'NONE', #5756, 'mechanical' ) ;
#9818 = DIRECTION ( 'NONE',  ( 0.000000000000000000, 0.000000000000000000, 1.000000000000000000 ) ) ;
#9819 = PRESENTATION_LAYER_ASSIGNMENT (  '', '', ( #9483 ) ) ;
#9820 = CARTESIAN_POINT ( 'NONE',  ( 7.874999999999916511, -0.001000000000001000089, -10.63990010960495880 ) ) ;
#9821 = CARTESIAN_POINT ( 'NONE',  ( -24.62111388750000884, 0.7812499990440845421, 10.19839929293505421 ) ) ;
#9822 = EDGE_CURVE ( 'NONE', #1765, #6566, #5000, .T. ) ;
#9823 = ORIENTED_EDGE ( 'NONE', *, *, #9706, .F. ) ;
#9824 = ORIENTED_EDGE ( 'NONE', *, *, #3348, .F. ) ;
#9825 = ORIENTED_EDGE ( 'NONE', *, *, #4600, .F. ) ;
#9826 =( GEOMETRIC_REPRESENTATION_CONTEXT ( 3 ) GLOBAL_UNCERTAINTY_ASSIGNED_CONTEXT ( ( #6817 ) ) GLOBAL_UNIT_ASSIGNED_CONTEXT ( ( #4912, #2404, #9052 ) ) REPRESENTATION_CONTEXT ( 'NONE', 'WORKASPACE' ) );
#9827 = ADVANCED_FACE ( 'NONE', ( #10188 ), #805, .T. ) ;
#9828 = CARTESIAN_POINT ( 'NONE',  ( -10.35533905932739174, 3.299999998088169129, 24.99999999999999289 ) ) ;
#9829 = FACE_OUTER_BOUND ( 'NONE', #3110, .T. ) ;
#9830 = AXIS2_PLACEMENT_3D ( 'NONE', #2834, #6233, #9595 ) ;
#9831 = CARTESIAN_POINT ( 'NONE',  ( -4.522825247065398226E-15, 0.9687499990440845421, 24.62111388750000174 ) ) ;
#9832 = VERTEX_POINT ( 'NONE', #7585 ) ;
#9833 = CARTESIAN_POINT ( 'NONE',  ( -6.312177826491033095, 10.00000000000000355, -3.066987298107852755 ) ) ;
#9834 =( LENGTH_UNIT ( ) NAMED_UNIT ( * ) SI_UNIT ( .MILLI., .METRE. ) );
#9835 = LINE ( 'NONE', #9635, #9674 ) ;
#9836 = PLANE ( 'NONE',  #7079 ) ;
#9837 = DIRECTION ( 'NONE',  ( -0.000000000000000000, -1.000000000000000000, -0.000000000000000000 ) ) ;
#9838 = CARTESIAN_POINT ( 'NONE',  ( 25.00000000000000000, 3.674999998088170017, -10.35533905932737753 ) ) ;
#9839 = EDGE_CURVE ( 'NONE', #716, #2686, #1684, .T. ) ;
#9840 = AXIS2_PLACEMENT_3D ( 'NONE', #10011, #9077, #5719 ) ;
#9841 = LINE ( 'NONE', #7521, #713 ) ;
#9842 = AXIS2_PLACEMENT_3D ( 'NONE', #8075, #5490, #2215 ) ;
#9843 = ORIENTED_EDGE ( 'NONE', *, *, #3926, .T. ) ;
#9844 = ORIENTED_EDGE ( 'NONE', *, *, #711, .F. ) ;
#9845 = CARTESIAN_POINT ( 'NONE',  ( -10.35533905932741128, 4.312500000000000888, -24.99999999999996803 ) ) ;
#9846 = CARTESIAN_POINT ( 'NONE',  ( 0.000000000000000000, 7.000000000000003553, 0.000000000000000000 ) ) ;
#9847 = CIRCLE ( 'NONE', #2089, 1.610000000000003872 ) ;
#9848 = DIRECTION ( 'NONE',  ( 1.000000000000000000, 0.000000000000000000, 0.000000000000000000 ) ) ;
#9849 = DIRECTION ( 'NONE',  ( -0.000000000000000000, -1.000000000000000000, -0.000000000000000000 ) ) ;
#9850 = CARTESIAN_POINT ( 'NONE',  ( -24.62111388750000174, 2.656249999044085097, -10.19839929293506131 ) ) ;
#9851 = CARTESIAN_POINT ( 'NONE',  ( 0.000000000000000000, 20.00000000000000355, 0.000000000000000000 ) ) ;
#9852 = ORIENTED_EDGE ( 'NONE', *, *, #8062, .T. ) ;
#9853 = ORIENTED_EDGE ( 'NONE', *, *, #3632, .F. ) ;
#9854 = ORIENTED_EDGE ( 'NONE', *, *, #8484, .T. ) ;
#9855 = AXIS2_PLACEMENT_3D ( 'NONE', #7090, #391, #5474 ) ;
#9856 = LINE ( 'NONE', #9704, #2678 ) ;
#9857 = EDGE_CURVE ( 'NONE', #1695, #6661, #1461, .T. ) ;
#9858 = CARTESIAN_POINT ( 'NONE',  ( 10.35533905932737930, 0.7999999980881692396, -25.00000000000000000 ) ) ;
#9859 = CARTESIAN_POINT ( 'NONE',  ( 27.60306914047445304, 97.85373563005803987, 5.000000000000000000 ) ) ;
#9860 = CARTESIAN_POINT ( 'NONE',  ( 0.000000000000000000, 7.000000000000003553, 0.000000000000000000 ) ) ;
#9861 = DIRECTION ( 'NONE',  ( -0.4999999999999887312, 0.000000000000000000, 0.8660254037844451469 ) ) ;
#9862 = VECTOR ( 'NONE', #4046, 1000.000000000000000 ) ;
#9863 = AXIS2_PLACEMENT_3D ( 'NONE', #4938, #7466, #1670 ) ;
#9864 = ORIENTED_EDGE ( 'NONE', *, *, #2873, .F. ) ;
#9865 = AXIS2_PLACEMENT_3D ( 'NONE', #9610, #3801, #3693 ) ;
#9866 = CARTESIAN_POINT ( 'NONE',  ( -1.500000000000000444, 88.00000000000001421, 1.499999999999999778 ) ) ;
#9867 = CARTESIAN_POINT ( 'NONE',  ( -7.276923788646446845, -0.001000000000001000089, 18.60400172474275848 ) ) ;
#9868 = CIRCLE ( 'NONE', #3892, 2.999999999999997335 ) ;
#9869 = CARTESIAN_POINT ( 'NONE',  ( 24.62111388750000174, 2.456249999044084475, -10.19839929293505776 ) ) ;
#9870 = ORIENTED_EDGE ( 'NONE', *, *, #6662, .T. ) ;
#9871 = DIRECTION ( 'NONE',  ( -1.000000000000000000, 0.000000000000000000, 0.000000000000000000 ) ) ;
#9872 = DIRECTION ( 'NONE',  ( 0.000000000000000000, 1.000000000000000000, 0.000000000000000000 ) ) ;
#9873 = CARTESIAN_POINT ( 'NONE',  ( -25.00000000000000000, 1.500000000000000000, -3.061616997868383043E-15 ) ) ;
#9874 = CARTESIAN_POINT ( 'NONE',  ( 1.507608415688466075E-15, 1.468749999044084431, -24.62111388750000174 ) ) ;
#9875 = ADVANCED_FACE ( 'NONE', ( #16 ), #10135, .T. ) ;
#9876 = EDGE_LOOP ( 'NONE', ( #8792, #8406, #3868, #2155 ) ) ;
#9877 = ORIENTED_EDGE ( 'NONE', *, *, #4709, .T. ) ;
#9878 = CIRCLE ( 'NONE', #10599, 2.149999999999999911 ) ;
#9879 = EDGE_CURVE ( 'NONE', #4112, #8744, #7826, .T. ) ;
#9880 = CARTESIAN_POINT ( 'NONE',  ( 24.62111388750000174, 0.4562499990440845310, -10.19839929293505776 ) ) ;
#9881 = FACE_OUTER_BOUND ( 'NONE', #5854, .T. ) ;
#9882 = CARTESIAN_POINT ( 'NONE',  ( 17.40975659021752620, 5.268749999044085364, 17.40975659021753330 ) ) ;
#9883 = VERTEX_POINT ( 'NONE', #4123 ) ;
#9884 = CARTESIAN_POINT ( 'NONE',  ( -3.499999999999921840, 20.00000000000000355, -6.062177826491114807 ) ) ;
#9885 = SURFACE_STYLE_USAGE ( .BOTH. , #9270 ) ;
#9886 = AXIS2_PLACEMENT_3D ( 'NONE', #9944, #7298, #7399 ) ;
#9887 = FACE_OUTER_BOUND ( 'NONE', #1458, .T. ) ;
#9888 = CARTESIAN_POINT ( 'NONE',  ( 82.32050807568876394, 89.28203230275514102, -5.000000000000000000 ) ) ;
#9889 = CARTESIAN_POINT ( 'NONE',  ( 0.000000000000000000, 20.00000000000000355, 0.000000000000000000 ) ) ;
#9890 = CARTESIAN_POINT ( 'NONE',  ( 25.00000000000000000, 0.6124999980881691286, 0.000000000000000000 ) ) ;
#9891 = EDGE_CURVE ( 'NONE', #3964, #7240, #10103, .T. ) ;
#9892 = EDGE_CURVE ( 'NONE', #5286, #2789, #415, .T. ) ;
#9893 = ORIENTED_EDGE ( 'NONE', *, *, #1814, .F. ) ;
#9894 = VERTEX_POINT ( 'NONE', #5013 ) ;
#9895 = EDGE_LOOP ( 'NONE', ( #1873, #7514, #140, #1538 ) ) ;
#9896 = ORIENTED_EDGE ( 'NONE', *, *, #7742, .F. ) ;
#9897 = UNCERTAINTY_MEASURE_WITH_UNIT (LENGTH_MEASURE( 1.000000000000000082E-05 ), #7566, 'distance_accuracy_value', 'NONE');
#9898 = ADVANCED_FACE ( 'NONE', ( #854 ), #4953, .F. ) ;
#9899 = AXIS2_PLACEMENT_3D ( 'NONE', #5561, #1460, #4737 ) ;
#9900 = FACE_OUTER_BOUND ( 'NONE', #4408, .T. ) ;
#9901 = DIRECTION ( 'NONE',  ( -0.000000000000000000, 1.000000000000000000, -0.000000000000000000 ) ) ;
#9902 = VERTEX_POINT ( 'NONE', #4221 ) ;
#9903 = AXIS2_PLACEMENT_3D ( 'NONE', #9314, #3400, #5139 ) ;
#9904 = DIRECTION ( 'NONE',  ( 0.000000000000000000, -1.000000000000000000, 0.000000000000000000 ) ) ;
#9905 = DIRECTION ( 'NONE',  ( 0.000000000000000000, 1.000000000000000000, 0.000000000000000000 ) ) ;
#9906 = DIRECTION ( 'NONE',  ( 0.8660254037844397068, 0.000000000000000000, -0.4999999999999979461 ) ) ;
#9907 = AXIS2_PLACEMENT_3D ( 'NONE', #2582, #10290, #2901 ) ;
#9908 = ORIENTED_EDGE ( 'NONE', *, *, #1380, .F. ) ;
#9909 = ADVANCED_FACE ( 'NONE', ( #7482 ), #3374, .F. ) ;
#9910 = ORIENTED_EDGE ( 'NONE', *, *, #1803, .F. ) ;
#9911 = VECTOR ( 'NONE', #5122, 1000.000000000000000 ) ;
#9912 = ORIENTED_EDGE ( 'NONE', *, *, #8407, .T. ) ;
#9913 = VECTOR ( 'NONE', #6393, 1000.000000000000114 ) ;
#9914 = CIRCLE ( 'NONE', #7116, 6.999999999999997335 ) ;
#9915 = FACE_OUTER_BOUND ( 'NONE', #637, .T. ) ;
#9916 = CARTESIAN_POINT ( 'NONE',  ( 0.1920286436967143240, 0.000000000000000000, 0.000000000000000000 ) ) ;
#9917 = CARTESIAN_POINT ( 'NONE',  ( -15.60400172474278158, -0.001000000000001000089, -12.47307621135316680 ) ) ;
#9918 = CARTESIAN_POINT ( 'NONE',  ( 0.000000000000000000, 28.00000000000000000, 0.000000000000000000 ) ) ;
#9919 = CARTESIAN_POINT ( 'NONE',  ( 0.000000000000000000, 10.00000000000000355, 0.000000000000000000 ) ) ;
#9920 = AXIS2_PLACEMENT_3D ( 'NONE', #10526, #365, #6587 ) ;
#9921 = AXIS2_PLACEMENT_3D ( 'NONE', #5035, #827, #4146 ) ;
#9922 = AXIS2_PLACEMENT_3D ( 'NONE', #744, #2442, #3437 ) ;
#9923 = ORIENTED_EDGE ( 'NONE', *, *, #6520, .T. ) ;
#9924 = AXIS2_PLACEMENT_3D ( 'NONE', #9918, #6009, #6728 ) ;
#9925 = SURFACE_STYLE_FILL_AREA ( #6564 ) ;
#9926 = DIRECTION ( 'NONE',  ( 0.000000000000000000, -1.000000000000000000, 0.000000000000000000 ) ) ;
#9927 = CARTESIAN_POINT ( 'NONE',  ( 17.40975659021752620, 2.268749999044084475, 17.40975659021753330 ) ) ;
#9928 = EDGE_LOOP ( 'NONE', ( #6498, #6172, #5202, #10007 ) ) ;
#9929 = DIRECTION ( 'NONE',  ( -0.000000000000000000, -0.000000000000000000, 1.000000000000000000 ) ) ;
#9930 = CARTESIAN_POINT ( 'NONE',  ( 0.000000000000000000, 29.50000000000000355, 0.000000000000000000 ) ) ;
#9931 = CARTESIAN_POINT ( 'NONE',  ( -0.1920286436967143240, 1.935951399190116865E-16, 6.975000000000007638 ) ) ;
#9932 = ORIENTED_EDGE ( 'NONE', *, *, #10533, .F. ) ;
#9933 = PLANE ( 'NONE',  #9921 ) ;
#9934 = CARTESIAN_POINT ( 'NONE',  ( 24.62111388749999108, 2.156249999044084653, 10.19839929293507730 ) ) ;
#9935 = VERTEX_POINT ( 'NONE', #9240 ) ;
#9936 = VECTOR ( 'NONE', #2294, 1000.000000000000000 ) ;
#9937 = ORIENTED_EDGE ( 'NONE', *, *, #2258, .F. ) ;
#9938 = VERTEX_POINT ( 'NONE', #1737 ) ;
#9939 = AXIS2_PLACEMENT_3D ( 'NONE', #6918, #2690, #6088 ) ;
#9940 = CARTESIAN_POINT ( 'NONE',  ( 10.35533905932737930, 2.799999998088169573, -25.00000000000000000 ) ) ;
#9941 = CARTESIAN_POINT ( 'NONE',  ( 9.874999999999895195, 28.00000000000000000, -17.10400172474272651 ) ) ;
#9942 = CARTESIAN_POINT ( 'NONE',  ( -10.19839929293505776, 1.531249999044084653, -24.62111388750000174 ) ) ;
#9943 = ORIENTED_EDGE ( 'NONE', *, *, #3539, .F. ) ;
#9944 = CARTESIAN_POINT ( 'NONE',  ( 0.000000000000000000, 88.00000000000001421, 0.000000000000000000 ) ) ;
#9945 = SURFACE_STYLE_FILL_AREA ( #5807 ) ;
#9946 = CARTESIAN_POINT ( 'NONE',  ( -6.062177826491100596, 20.00000000000000355, 3.499999999999942712 ) ) ;
#9947 = DIRECTION ( 'NONE',  ( 0.000000000000000000, -1.000000000000000000, 2.775557561562888270E-17 ) ) ;
#9948 = DIRECTION ( 'NONE',  ( -0.000000000000000000, -1.000000000000000000, -0.000000000000000000 ) ) ;
#9949 = DIRECTION ( 'NONE',  ( -0.000000000000000000, -1.000000000000000000, -0.000000000000000000 ) ) ;
#9950 = VERTEX_POINT ( 'NONE', #2547 ) ;
#9951 = VERTEX_POINT ( 'NONE', #3258 ) ;
#9952 = EDGE_CURVE ( 'NONE', #5793, #6120, #6716, .T. ) ;
#9953 = ADVANCED_FACE ( 'NONE', ( #6606 ), #10913, .T. ) ;
#9954 = CARTESIAN_POINT ( 'NONE',  ( -10.19839929293507552, 3.081249999044084475, 24.62111388749999463 ) ) ;
#9955 = CARTESIAN_POINT ( 'NONE',  ( -24.62111388750000174, 0.7187499990440845421, -3.015216831376932151E-15 ) ) ;
#9956 = EDGE_CURVE ( 'NONE', #7963, #7237, #2393, .T. ) ;
#9957 = SURFACE_SIDE_STYLE ('',( #908 ) ) ;
#9958 = EDGE_LOOP ( 'NONE', ( #10555, #1491, #3690, #5772 ) ) ;
#9959 = CARTESIAN_POINT ( 'NONE',  ( 3.644491357022514588, 19.66631150450990262, -5.978755702618546053 ) ) ;
#9960 = CARTESIAN_POINT ( 'NONE',  ( -5.276923788646495694, 25.00000000000000000, 15.13990010960498012 ) ) ;
#9961 = DIRECTION ( 'NONE',  ( 0.000000000000000000, 1.000000000000000000, 0.000000000000000000 ) ) ;
#9962 = CARTESIAN_POINT ( 'NONE',  ( -10.19839929293507552, 0.9062499990440844311, 24.62111388749999463 ) ) ;
#9963 = DIRECTION ( 'NONE',  ( -0.000000000000000000, 0.000000000000000000, -1.000000000000000000 ) ) ;
#9964 = EDGE_CURVE ( 'NONE', #57, #9754, #10139, .T. ) ;
#9965 = ORIENTED_EDGE ( 'NONE', *, *, #5037, .F. ) ;
#9966 = VERTEX_POINT ( 'NONE', #1090 ) ;
#9967 = VERTEX_POINT ( 'NONE', #2719 ) ;
#9968 = ORIENTED_EDGE ( 'NONE', *, *, #9236, .F. ) ;
#9969 = ORIENTED_EDGE ( 'NONE', *, *, #10386, .F. ) ;
#9970 = EDGE_CURVE ( 'NONE', #2208, #9105, #7825, .T. ) ;
#9971 = LINE ( 'NONE', #4231, #9911 ) ;
#9972 = CARTESIAN_POINT ( 'NONE',  ( -4.592425496802574367E-15, 0.7500000000000000000, 25.00000000000000000 ) ) ;
#9973 = DIRECTION ( 'NONE',  ( 0.000000000000000000, -1.000000000000000000, 0.000000000000000000 ) ) ;
#9974 = DIRECTION ( 'NONE',  ( 0.000000000000000000, 0.000000000000000000, 1.000000000000000000 ) ) ;
#9975 = CARTESIAN_POINT ( 'NONE',  ( 18.31891771041502537, 4.999999999999998224, 16.72517935659742960 ) ) ;
#9976 = EDGE_CURVE ( 'NONE', #5308, #10414, #5239, .T. ) ;
#9977 = ORIENTED_EDGE ( 'NONE', *, *, #9964, .F. ) ;
#9978 = EDGE_LOOP ( 'NONE', ( #7071, #6131, #8452, #4924 ) ) ;
#9979 = LINE ( 'NONE', #3114, #8598 ) ;
#9980 = FACE_OUTER_BOUND ( 'NONE', #5134, .T. ) ;
#9981 = ORIENTED_EDGE ( 'NONE', *, *, #8143, .T. ) ;
#9982 = DIRECTION ( 'NONE',  ( 0.000000000000000000, 0.000000000000000000, -1.000000000000000000 ) ) ;
#9983 = APPLICATION_PROTOCOL_DEFINITION ( 'draft international standard', 'automotive_design', 1998, #8930 ) ;
#9984 = CYLINDRICAL_SURFACE ( 'NONE', #7469, 27.91176187412963117 ) ;
#9985 = DIRECTION ( 'NONE',  ( -0.000000000000000000, -1.000000000000000000, -0.000000000000000000 ) ) ;
#9986 = CARTESIAN_POINT ( 'NONE',  ( -24.62111388750000174, 2.656249999044085097, -10.19839929293506131 ) ) ;
#9987 = ORIENTED_EDGE ( 'NONE', *, *, #1455, .F. ) ;
#9988 = VERTEX_POINT ( 'NONE', #255 ) ;
#9989 = CARTESIAN_POINT ( 'NONE',  ( -10.19839929293505776, 0.7062499990440844755, -24.62111388750000174 ) ) ;
#9990 = DIRECTION ( 'NONE',  ( 0.000000000000000000, 0.000000000000000000, 1.000000000000000000 ) ) ;
#9991 = CARTESIAN_POINT ( 'NONE',  ( 10.19839929293505953, 3.406249999044085097, -24.62111388750000174 ) ) ;
#9992 = DIRECTION ( 'NONE',  ( 0.4999999999999977796, 0.000000000000000000, -0.8660254037844399289 ) ) ;
#9993 = EDGE_LOOP ( 'NONE', ( #3859, #6191, #7681, #1260 ) ) ;
#9994 = CARTESIAN_POINT ( 'NONE',  ( 1.499999999999999556, 83.00000000000000000, -1.500000000000000222 ) ) ;
#9995 =( NAMED_UNIT ( * ) PLANE_ANGLE_UNIT ( ) SI_UNIT ( $, .RADIAN. ) );
#9996 =( NAMED_UNIT ( * ) SI_UNIT ( $, .STERADIAN. ) SOLID_ANGLE_UNIT ( ) );
#9997 = SHAPE_REPRESENTATION ( 'socket set screw cone point_iso_ISO 4027 - M4 x 16-N', ( #7040 ), #8779 ) ;
#9998 = EDGE_CURVE ( 'NONE', #10484, #7237, #1194, .T. ) ;
#9999 = CYLINDRICAL_SURFACE ( 'NONE', #3679, 25.00000000000000000 ) ;
#10000 = DIRECTION ( 'NONE',  ( 0.4999999999999947820, 0.000000000000000000, -0.8660254037844417052 ) ) ;
#10001 = DIRECTION ( 'NONE',  ( -0.000000000000000000, -1.000000000000000000, -0.000000000000000000 ) ) ;
#10002 = CARTESIAN_POINT ( 'NONE',  ( -1.500000000000000444, 83.00000000000000000, 1.499999999999999778 ) ) ;
#10003 = AXIS2_PLACEMENT_3D ( 'NONE', #7499, #10877, #3276 ) ;
#10004 = PRODUCT_RELATED_PRODUCT_CATEGORY ( 'part', '', ( #4613 ) ) ;
#10005 = ORIENTED_EDGE ( 'NONE', *, *, #5056, .T. ) ;
#10006 = ORIENTED_EDGE ( 'NONE', *, *, #7486, .F. ) ;
#10007 = ORIENTED_EDGE ( 'NONE', *, *, #9956, .F. ) ;
#10008 = CLOSED_SHELL ( 'NONE', ( #10936, #8008, #9647, #7264, #9079, #1143, #467, #7153, #1058, #8634, #5782, #177, #3064, #8270, #3819, #5633, #3718, #6155, #8911, #4716, #3408, #3211, #4968, #1940, #6729, #6138, #9147, #4175, #10920, #7075, #7376, #3272, #2999, #2813 ) ) ;
#10009 = CARTESIAN_POINT ( 'NONE',  ( 17.40975659021752975, 0.5187499990440845865, -17.40975659021752975 ) ) ;
#10010 = DIRECTION ( 'NONE',  ( -0.4999999999999888423, 0.000000000000000000, -0.8660254037844449249 ) ) ;
#10011 = CARTESIAN_POINT ( 'NONE',  ( 0.000000000000000000, 20.00000000000000355, 0.000000000000000000 ) ) ;
#10012 = MECHANICAL_DESIGN_GEOMETRIC_PRESENTATION_REPRESENTATION (  '', ( #7728 ), #1036 ) ;
#10013 = PLANE ( 'NONE',  #4606 ) ;
#10014 = LINE ( 'NONE', #4951, #10278 ) ;
#10015 = CARTESIAN_POINT ( 'NONE',  ( 10.35533905932734733, 4.799999998088170905, -25.00000000000004263 ) ) ;
#10016 = AXIS2_PLACEMENT_3D ( 'NONE', #2477, #3135, #5706 ) ;
#10017 = CARTESIAN_POINT ( 'NONE',  ( -24.62111388750000174, 0.7187499990440845421, -3.015216831376932151E-15 ) ) ;
#10018 = DIRECTION ( 'NONE',  ( -0.000000000000000000, 1.000000000000000000, -0.000000000000000000 ) ) ;
#10019 = EDGE_CURVE ( 'NONE', #2423, #4873, #7000, .T. ) ;
#10020 = VERTEX_POINT ( 'NONE', #6056 ) ;
#10021 = ORIENTED_EDGE ( 'NONE', *, *, #8815, .T. ) ;
#10022 = ORIENTED_EDGE ( 'NONE', *, *, #439, .T. ) ;
#10023 = CIRCLE ( 'NONE', #337, 1.610000000000003872 ) ;
#10024 = EDGE_CURVE ( 'NONE', #5725, #3304, #9535, .T. ) ;
#10025 = CARTESIAN_POINT ( 'NONE',  ( 0.000000000000000000, 28.00000000000000000, 0.000000000000000000 ) ) ;
#10026 = DIRECTION ( 'NONE',  ( 0.000000000000000000, 1.000000000000000000, 0.000000000000000000 ) ) ;
#10027 = CYLINDRICAL_SURFACE ( 'NONE', #9762, 6.999999999999997335 ) ;
#10028 = LINE ( 'NONE', #9806, #5198 ) ;
#10029 = DIRECTION ( 'NONE',  ( 1.000000000000000000, 0.000000000000000000, 0.000000000000000000 ) ) ;
#10030 = EDGE_CURVE ( 'NONE', #8026, #7707, #5344, .T. ) ;
#10031 = EDGE_LOOP ( 'NONE', ( #2845, #67, #5430, #8261, #1445 ) ) ;
#10032 = ORIENTED_EDGE ( 'NONE', *, *, #3014, .F. ) ;
#10033 = EDGE_CURVE ( 'NONE', #9593, #8354, #10245, .T. ) ;
#10034 = DIRECTION ( 'NONE',  ( 0.000000000000000000, 0.000000000000000000, 1.000000000000000000 ) ) ;
#10035 = LINE ( 'NONE', #8377, #6381 ) ;
#10036 = FILL_AREA_STYLE_COLOUR ( '', #10715 ) ;
#10037 = ORIENTED_EDGE ( 'NONE', *, *, #3833, .F. ) ;
#10038 = DIRECTION ( 'NONE',  ( 0.000000000000000000, 0.000000000000000000, 1.000000000000000000 ) ) ;
#10039 = APPLICATION_PROTOCOL_DEFINITION ( 'draft international standard', 'automotive_design', 1998, #2156 ) ;
#10040 = LINE ( 'NONE', #4191, #6420 ) ;
#10041 = ORIENTED_EDGE ( 'NONE', *, *, #7197, .F. ) ;
#10042 = DIRECTION ( 'NONE',  ( 0.000000000000000000, -1.000000000000000000, 0.000000000000000000 ) ) ;
#10043 = CARTESIAN_POINT ( 'NONE',  ( -10.19839929293507375, 2.906249999044085541, 24.62111388749999108 ) ) ;
#10044 = EDGE_LOOP ( 'NONE', ( #6635, #7589, #2031, #3615 ) ) ;
#10045 = ORIENTED_EDGE ( 'NONE', *, *, #94, .F. ) ;
#10046 = VECTOR ( 'NONE', #7903, 1000.000000000000000 ) ;
#10047 = VECTOR ( 'NONE', #6594, 1000.000000000000114 ) ;
#10048 = EDGE_CURVE ( 'NONE', #3835, #6439, #9048, .T. ) ;
#10049 = CARTESIAN_POINT ( 'NONE',  ( 24.62111388750000174, 4.456249999044084475, -10.19839929293505776 ) ) ;
#10050 = DIRECTION ( 'NONE',  ( 0.000000000000000000, 1.000000000000000000, 0.000000000000000000 ) ) ;
#10051 = CARTESIAN_POINT ( 'NONE',  ( -17.40975659021753330, 1.843749999044084653, 17.40975659021752975 ) ) ;
#10052 = DIRECTION ( 'NONE',  ( 1.445602896647339163E-16, 0.000000000000000000, 1.000000000000000000 ) ) ;
#10053 = ORIENTED_EDGE ( 'NONE', *, *, #2748, .F. ) ;
#10054 = SURFACE_STYLE_FILL_AREA ( #1665 ) ;
#10055 = CARTESIAN_POINT ( 'NONE',  ( 25.00000000000000000, 1.674999998088169351, -10.35533905932737753 ) ) ;
#10056 = CARTESIAN_POINT ( 'NONE',  ( -5.276923788646812774, 25.00000000000000000, -15.13990010960486821 ) ) ;
#10057 = CARTESIAN_POINT ( 'NONE',  ( 0.000000000000000000, 31.00000000000000000, 0.000000000000000000 ) ) ;
#10058 = CARTESIAN_POINT ( 'NONE',  ( -7.276923788646446845, -0.001000000000001000089, 18.60400172474275848 ) ) ;
#10059 = VECTOR ( 'NONE', #1043, 1000.000000000000114 ) ;
#10060 = AXIS2_PLACEMENT_3D ( 'NONE', #3528, #2575, #2696 ) ;
#10061 = APPLICATION_CONTEXT ( 'automotive_design' ) ;
#10062 = VERTEX_POINT ( 'NONE', #6886 ) ;
#10063 = EDGE_LOOP ( 'NONE', ( #7631, #6835, #3697, #9893 ) ) ;
#10064 = EDGE_LOOP ( 'NONE', ( #8034, #9296, #1335, #4331 ) ) ;
#10065 = VERTEX_POINT ( 'NONE', #7764 ) ;
#10066 = CIRCLE ( 'NONE', #7245, 2.999999999999997335 ) ;
#10067 =( BOUNDED_SURFACE ( )  B_SPLINE_SURFACE ( 1, 2, ( 
 ( #2035, #5411, #1355, #1509, #6657, #1462, #3098, #4122, #10017, #743, #5823, #9962, #10690, #6715, #4063, #1624, #2441, #10739, #9185, #3152, #9131, #4008, #8196, #4891, #6547, #7311, #8243, #4849, #10859, #5765, #7531, #629, #5012, #5064, #8363, #3206, #804, #2340, #6493, #9850, #2287, #4170, #3257, #7481, #5722, #10073, #8301, #9081, #686, #10912, #7421, #3312, #5887, #7362, #2488, #9239, #1683, #2392, #8411, #853, #1564, #5668, #9028, #6605, #10802, #5292, #1030, #4404, #1796, #9354, #5177, #2770, #7646, #8641, #10187, #1089, #5997, #10134, #4464, #15, #7763 ),
 ( #6777, #2546, #8466, #2718, #2659, #5939, #6170, #135, #7824, #3555, #80, #10308, #3436, #5238, #4282, #5111, #8528, #2602, #4220, #3498, #9290, #195, #8582, #254, #6947, #9534, #1973, #5343, #8701, #1736, #9640, #6228, #358, #7980, #2170, #4683, #10569, #7157, #1151, #2115, #8857, #4726, #1894, #6039, #10291, #3599, #118, #5274, #8624, #6932, #4384, #1070, #2707, #7747, #6987, #6103, #8567, #175, #4445, #9462, #5159, #1842, #5224, #1015, #8508, #2643, #962, #4327, #7689, #3478, #9400, #6867, #10226, #303, #7928, #7880, #1149, #2658, #6884, #7762, #1908 ) ),
 .UNSPECIFIED., .F., .F., .F. ) 
 B_SPLINE_SURFACE_WITH_KNOTS ( ( 2, 2 ),
 ( 3, 2, 2, 2, 2, 2, 2, 2, 2, 2, 2, 2, 2, 2, 2, 2, 2, 2, 2, 2, 2, 2, 2, 2, 2, 2, 2, 2, 2, 2, 2, 2, 2, 2, 2, 2, 2, 2, 2, 2, 3 ),
 ( 0.000000000000000000, 1.000000000000000000 ),
 ( 0.000000000000000000, 0.02500000000000000139, 0.05000000000000000278, 0.07499999999999999722, 0.1000000000000000056, 0.1250000000000000000, 0.1499999999999999944, 0.1749999999999999889, 0.2000000000000000111, 0.2250000000000000056, 0.2500000000000000000, 0.2750000000000000222, 0.2999999999999999889, 0.3250000000000000111, 0.3499999999999999778, 0.3750000000000000000, 0.4000000000000000222, 0.4249999999999999889, 0.4500000000000000111, 0.4749999999999999778, 0.5000000000000000000, 0.5250000000000000222, 0.5500000000000000444, 0.5749999999999999556, 0.5999999999999999778, 0.6250000000000000000, 0.6500000000000000222, 0.6750000000000000444, 0.6999999999999999556, 0.7249999999999999778, 0.7500000000000000000, 0.7750000000000000222, 0.8000000000000000444, 0.8249999999999999556, 0.8499999999999999778, 0.8750000000000000000, 0.9000000000000000222, 0.9250000000000000444, 0.9499999999999999556, 0.9749999999999999778, 1.000000000000000000 ),
 .UNSPECIFIED. ) 
 GEOMETRIC_REPRESENTATION_ITEM ( )  RATIONAL_B_SPLINE_SURFACE ( (
 ( 1.000000000000000000, 0.9238795325112867385, 1.000000000000000000, 0.9238795325112867385, 1.000000000000000000, 0.9238795325112867385, 1.000000000000000000, 0.9238795325112867385, 1.000000000000000000, 0.9238795325112867385, 1.000000000000000000, 0.9238795325112867385, 1.000000000000000000, 0.9238795325112867385, 1.000000000000000000, 0.9238795325112867385, 1.000000000000000000, 0.9238795325112867385, 1.000000000000000000, 0.9238795325112867385, 1.000000000000000000, 0.9238795325112867385, 1.000000000000000000, 0.9238795325112867385, 1.000000000000000000, 0.9238795325112867385, 1.000000000000000000, 0.9238795325112867385, 1.000000000000000000, 0.9238795325112867385, 1.000000000000000000, 0.9238795325112867385, 1.000000000000000000, 0.9238795325112867385, 1.000000000000000000, 0.9238795325112867385, 1.000000000000000000, 0.9238795325112867385, 1.000000000000000000, 0.9238795325112867385, 1.000000000000000000, 0.9238795325112867385, 1.000000000000000000, 0.9238795325112867385, 1.000000000000000000, 0.9238795325112867385, 1.000000000000000000, 0.9238795325112867385, 1.000000000000000000, 0.9238795325112867385, 1.000000000000000000, 0.9238795325112867385, 1.000000000000000000, 0.9238795325112867385, 1.000000000000000000, 0.9238795325112867385, 1.000000000000000000, 0.9238795325112867385, 1.000000000000000000, 0.9238795325112867385, 1.000000000000000000, 0.9238795325112867385, 1.000000000000000000, 0.9238795325112867385, 1.000000000000000000, 0.9238795325112867385, 1.000000000000000000, 0.9238795325112867385, 1.000000000000000000, 0.9238795325112867385, 1.000000000000000000, 0.9238795325112867385, 1.000000000000000000, 0.9238795325112867385, 1.000000000000000000, 0.9238795325112867385, 1.000000000000000000, 0.9238795325112867385, 1.000000000000000000, 0.9238795325112867385, 1.000000000000000000),
 ( 1.000000000000000000, 0.9238795325112867385, 1.000000000000000000, 0.9238795325112867385, 1.000000000000000000, 0.9238795325112867385, 1.000000000000000000, 0.9238795325112867385, 1.000000000000000000, 0.9238795325112867385, 1.000000000000000000, 0.9238795325112867385, 1.000000000000000000, 0.9238795325112867385, 1.000000000000000000, 0.9238795325112867385, 1.000000000000000000, 0.9238795325112867385, 1.000000000000000000, 0.9238795325112867385, 1.000000000000000000, 0.9238795325112867385, 1.000000000000000000, 0.9238795325112867385, 1.000000000000000000, 0.9238795325112867385, 1.000000000000000000, 0.9238795325112867385, 1.000000000000000000, 0.9238795325112867385, 1.000000000000000000, 0.9238795325112867385, 1.000000000000000000, 0.9238795325112867385, 1.000000000000000000, 0.9238795325112867385, 1.000000000000000000, 0.9238795325112867385, 1.000000000000000000, 0.9238795325112867385, 1.000000000000000000, 0.9238795325112867385, 1.000000000000000000, 0.9238795325112867385, 1.000000000000000000, 0.9238795325112867385, 1.000000000000000000, 0.9238795325112867385, 1.000000000000000000, 0.9238795325112867385, 1.000000000000000000, 0.9238795325112867385, 1.000000000000000000, 0.9238795325112867385, 1.000000000000000000, 0.9238795325112867385, 1.000000000000000000, 0.9238795325112867385, 1.000000000000000000, 0.9238795325112867385, 1.000000000000000000, 0.9238795325112867385, 1.000000000000000000, 0.9238795325112867385, 1.000000000000000000, 0.9238795325112867385, 1.000000000000000000, 0.9238795325112867385, 1.000000000000000000, 0.9238795325112867385, 1.000000000000000000, 0.9238795325112867385, 1.000000000000000000, 0.9238795325112867385, 1.000000000000000000, 0.9238795325112867385, 1.000000000000000000, 0.9238795325112867385, 1.000000000000000000, 0.9238795325112867385, 1.000000000000000000) ) ) 
 REPRESENTATION_ITEM ( '' )  SURFACE ( )  );
#10068 = CARTESIAN_POINT ( 'NONE',  ( 1.507608415688466075E-15, 1.643749999044084475, -24.62111388750000174 ) ) ;
#10069 = CARTESIAN_POINT ( 'NONE',  ( -10.19839929293507552, 0.9062499990440844311, 24.62111388749999463 ) ) ;
#10070 = DIRECTION ( 'NONE',  ( 0.000000000000000000, 1.000000000000000000, 0.000000000000000000 ) ) ;
#10071 = CARTESIAN_POINT ( 'NONE',  ( -12.67266974794317491, 5.000000000000000888, 21.23116648297597209 ) ) ;
#10072 = LINE ( 'NONE', #7584, #7605 ) ;
#10073 = CARTESIAN_POINT ( 'NONE',  ( 10.19839929293506486, 3.031249999044084653, 24.62111388749999819 ) ) ;
#10074 = CARTESIAN_POINT ( 'NONE',  ( 0.000000000000000000, 5.000000000000000000, 0.000000000000000000 ) ) ;
#10075 = ORIENTED_EDGE ( 'NONE', *, *, #8813, .T. ) ;
#10076 = ORIENTED_EDGE ( 'NONE', *, *, #9013, .T. ) ;
#10077 = ORIENTED_EDGE ( 'NONE', *, *, #335, .F. ) ;
#10078 = VECTOR ( 'NONE', #2074, 1000.000000000000114 ) ;
#10079 = ORIENTED_EDGE ( 'NONE', *, *, #1715, .F. ) ;
#10080 = CYLINDRICAL_SURFACE ( 'NONE', #9045, 12.77350269189627063 ) ;
#10081 = ADVANCED_FACE ( 'NONE', ( #5293 ), #5365, .T. ) ;
#10082 = CARTESIAN_POINT ( 'NONE',  ( 0.000000000000000000, 7.000000000000003553, 0.000000000000000000 ) ) ;
#10083 = DIRECTION ( 'NONE',  ( 0.000000000000000000, 0.000000000000000000, -1.000000000000000000 ) ) ;
#10084 = CARTESIAN_POINT ( 'NONE',  ( 3.058047309049977791, 10.00000000000000355, 6.296693311223928724 ) ) ;
#10085 = CARTESIAN_POINT ( 'NONE',  ( 0.5000000000000001110, 10.00000000000000355, 6.982120021884469452 ) ) ;
#10086 = EDGE_CURVE ( 'NONE', #5017, #3638, #976, .T. ) ;
#10087 = ORIENTED_EDGE ( 'NONE', *, *, #5051, .T. ) ;
#10088 = VECTOR ( 'NONE', #10815, 1000.000000000000000 ) ;
#10089 = CARTESIAN_POINT ( 'NONE',  ( 25.00000000000000000, 5.000000000000000000, 0.000000000000000000 ) ) ;
#10090 = CARTESIAN_POINT ( 'NONE',  ( 9.474358296526961709, 10.00000000000000355, -2.857142857142823011 ) ) ;
#10091 = DIRECTION ( 'NONE',  ( -0.000000000000000000, -1.000000000000000000, -0.000000000000000000 ) ) ;
#10092 = ADVANCED_FACE ( 'NONE', ( #6171 ), #3612, .F. ) ;
#10093 = CARTESIAN_POINT ( 'NONE',  ( 0.000000000000000000, 10.10000000000000497, 0.000000000000000000 ) ) ;
#10094 = ORIENTED_EDGE ( 'NONE', *, *, #2201, .F. ) ;
#10095 = EDGE_CURVE ( 'NONE', #7535, #10522, #7998, .T. ) ;
#10096 = VECTOR ( 'NONE', #7835, 1000.000000000000000 ) ;
#10097 = DIRECTION ( 'NONE',  ( 3.708321773340234242E-15, 0.000000000000000000, 1.000000000000000000 ) ) ;
#10098 = EDGE_CURVE ( 'NONE', #4873, #1851, #8757, .T. ) ;
#10099 = VECTOR ( 'NONE', #3175, 1000.000000000000000 ) ;
#10100 = CARTESIAN_POINT ( 'NONE',  ( 14.00000000000000533, 0.000000000000000000, 0.000000000000000000 ) ) ;
#10101 = CARTESIAN_POINT ( 'NONE',  ( -25.00000000000001066, 5.174999998088170017, 10.35533905932737397 ) ) ;
#10102 = CARTESIAN_POINT ( 'NONE',  ( 3.924072712834459686, 10.00000000000000355, -5.796693311223905631 ) ) ;
#10103 = CIRCLE ( 'NONE', #3383, 25.00000000000000000 ) ;
#10104 = EDGE_CURVE ( 'NONE', #7190, #7313, #2660, .T. ) ;
#10105 = VERTEX_POINT ( 'NONE', #3605 ) ;
#10106 = AXIS2_PLACEMENT_3D ( 'NONE', #1838, #1777, #1713 ) ;
#10107 = ORIENTED_EDGE ( 'NONE', *, *, #6080, .F. ) ;
#10108 = CIRCLE ( 'NONE', #1468, 2.000000000000000000 ) ;
#10109 = DIRECTION ( 'NONE',  ( -0.4330127018922225179, -0.8660254037844380415, 0.2499999999999964473 ) ) ;
#10110 = DIRECTION ( 'NONE',  ( 0.2500000000000041078, 0.8660254037844380415, -0.4330127018922181881 ) ) ;
#10111 = LINE ( 'NONE', #6696, #30 ) ;
#10112 = ORIENTED_EDGE ( 'NONE', *, *, #1478, .T. ) ;
#10113 = EDGE_CURVE ( 'NONE', #4640, #8620, #2009, .T. ) ;
#10114 = DIRECTION ( 'NONE',  ( -0.000000000000000000, -1.000000000000000000, -0.000000000000000000 ) ) ;
#10115 = DIRECTION ( 'NONE',  ( 0.000000000000000000, 0.000000000000000000, -1.000000000000000000 ) ) ;
#10116 = FACE_OUTER_BOUND ( 'NONE', #9133, .T. ) ;
#10117 = VECTOR ( 'NONE', #1474, 1000.000000000000000 ) ;
#10118 = DIRECTION ( 'NONE',  ( 0.000000000000000000, 1.000000000000000000, 0.000000000000000000 ) ) ;
#10119 = PLANE ( 'NONE',  #8274 ) ;
#10120 = EDGE_CURVE ( 'NONE', #6566, #2789, #10818, .T. ) ;
#10121 = AXIS2_PLACEMENT_3D ( 'NONE', #9917, #2353, #6406 ) ;
#10122 = ORIENTED_EDGE ( 'NONE', *, *, #3066, .F. ) ;
#10123 = ORIENTED_EDGE ( 'NONE', *, *, #247, .T. ) ;
#10124 = ORIENTED_EDGE ( 'NONE', *, *, #574, .F. ) ;
#10125 = ORIENTED_EDGE ( 'NONE', *, *, #3770, .F. ) ;
#10126 = DIRECTION ( 'NONE',  ( 0.000000000000000000, 0.000000000000000000, -1.000000000000000000 ) ) ;
#10127 = CARTESIAN_POINT ( 'NONE',  ( -24.62111388750000174, 0.7187499990440845421, -3.015216831376932151E-15 ) ) ;
#10128 = CARTESIAN_POINT ( 'NONE',  ( 24.62111388750000174, 0.4562499990440845310, -10.19839929293505776 ) ) ;
#10129 = CARTESIAN_POINT ( 'NONE',  ( -25.00000000000001421, 0.5625000000000001110, 10.35533905932737397 ) ) ;
#10130 = DIRECTION ( 'NONE',  ( 0.000000000000000000, -1.000000000000000000, 0.000000000000000000 ) ) ;
#10131 = VERTEX_POINT ( 'NONE', #5282 ) ;
#10132 = CARTESIAN_POINT ( 'NONE',  ( 67.32050807568876394, 89.28203230275514102, -5.000000000000000000 ) ) ;
#10133 = CARTESIAN_POINT ( 'NONE',  ( 1.500000000000001332, 1.013986724829958402E-15, 6.750000000000000000 ) ) ;
#10134 = CARTESIAN_POINT ( 'NONE',  ( 10.19839929293506486, 5.031249999044083765, 24.62111388749999819 ) ) ;
#10135 = CYLINDRICAL_SURFACE ( 'NONE', #8330, 25.00000000000000000 ) ;
#10136 = EDGE_LOOP ( 'NONE', ( #4500, #9159, #10706 ) ) ;
#10137 = EDGE_LOOP ( 'NONE', ( #142, #5345, #6518, #3 ) ) ;
#10138 = VERTEX_POINT ( 'NONE', #2712 ) ;
#10139 =( BOUNDED_CURVE ( )  B_SPLINE_CURVE ( 2, ( #913, #4283, #7647, #5178, #81, #6828, #197, #1974, #1909 ),
 .UNSPECIFIED., .F., .F. ) 
 B_SPLINE_CURVE_WITH_KNOTS ( ( 3, 2, 2, 2, 3 ),
 ( 0.4500000000000000111, 0.4749999999999999778, 0.5000000000000000000, 0.5250000000000000222, 0.5500000000000000444 ),
 .UNSPECIFIED. ) 
 CURVE ( )  GEOMETRIC_REPRESENTATION_ITEM ( )  RATIONAL_B_SPLINE_CURVE ( ( 1.000000000000000000, 0.9238795325112867385, 1.000000000000000000, 0.9238795325112867385, 1.000000000000000000, 0.9238795325112867385, 1.000000000000000000, 0.9238795325112867385, 1.000000000000000000 ) ) 
 REPRESENTATION_ITEM ( '' )  );
#10140 = DIRECTION ( 'NONE',  ( 0.000000000000000000, 0.000000000000000000, 1.000000000000000000 ) ) ;
#10141 = ORIENTED_EDGE ( 'NONE', *, *, #8335, .T. ) ;
#10142 = CARTESIAN_POINT ( 'NONE',  ( 17.67766952966368521, 1.875000000000000000, 17.67766952966369232 ) ) ;
#10143 = CARTESIAN_POINT ( 'NONE',  ( 10.35533905932742016, 4.812499999999999112, 24.99999999999996447 ) ) ;
#10144 = FACE_OUTER_BOUND ( 'NONE', #3102, .T. ) ;
#10145 = CARTESIAN_POINT ( 'NONE',  ( 25.00000000000000000, 5.000000000000000000, 0.000000000000000000 ) ) ;
#10146 = PRODUCT_DEFINITION ( 'UNKNOWN', '', #7061, #733 ) ;
#10147 = VERTEX_POINT ( 'NONE', #9469 ) ;
#10148 = FACE_OUTER_BOUND ( 'NONE', #7250, .T. ) ;
#10149 = DIRECTION ( 'NONE',  ( -0.000000000000000000, -1.000000000000000000, -0.000000000000000000 ) ) ;
#10150 = DIRECTION ( 'NONE',  ( 0.000000000000000000, 0.000000000000000000, 1.000000000000000000 ) ) ;
#10151 = ORIENTED_EDGE ( 'NONE', *, *, #3320, .F. ) ;
#10152 = DIRECTION ( 'NONE',  ( 0.000000000000000000, 0.000000000000000000, -1.000000000000000000 ) ) ;
#10153 = ITEM_DEFINED_TRANSFORMATION ( 'NONE', 'NONE', #5639,  #7040 ) ;
#10154 = DIRECTION ( 'NONE',  ( 0.000000000000000000, 0.000000000000000000, 1.000000000000000000 ) ) ;
#10155 = CARTESIAN_POINT ( 'NONE',  ( 25.00000000000000000, 0.3062499990440845643, 0.000000000000000000 ) ) ;
#10156 = DIRECTION ( 'NONE',  ( 0.000000000000000000, 0.000000000000000000, -1.000000000000000000 ) ) ;
#10157 = VERTEX_POINT ( 'NONE', #1847 ) ;
#10158 = EDGE_CURVE ( 'NONE', #8118, #5055, #6059, .T. ) ;
#10159 = ORIENTED_EDGE ( 'NONE', *, *, #4743, .F. ) ;
#10160 = CARTESIAN_POINT ( 'NONE',  ( 10.19839929293506486, 1.206249999044084698, 24.62111388749999819 ) ) ;
#10161 = CARTESIAN_POINT ( 'NONE',  ( -10.19839929293507552, 3.081249999044084475, 24.62111388749999463 ) ) ;
#10162 = CARTESIAN_POINT ( 'NONE',  ( 1.500000000000001332, 5.100000000000004974, 0.000000000000000000 ) ) ;
#10163 = CARTESIAN_POINT ( 'NONE',  ( 3.924072712834459686, 19.03096903053429756, -5.796693311223905631 ) ) ;
#10164 = CARTESIAN_POINT ( 'NONE',  ( -1.500000000000001332, -2.053912595556539452E-16, -7.400000000000007461 ) ) ;
#10165 = VERTEX_POINT ( 'NONE', #7637 ) ;
#10166 = DIRECTION ( 'NONE',  ( -0.000000000000000000, -1.000000000000000000, -0.000000000000000000 ) ) ;
#10167 = EDGE_CURVE ( 'NONE', #8513, #5192, #6048, .T. ) ;
#10168 = DIRECTION ( 'NONE',  ( 0.000000000000000000, -2.775557561562887961E-17, -1.000000000000000000 ) ) ;
#10169 = CARTESIAN_POINT ( 'NONE',  ( 0.000000000000000000, 20.00000000000000355, 0.000000000000000000 ) ) ;
#10170 = CARTESIAN_POINT ( 'NONE',  ( 19.75000000000001066, 25.00000000000000000, 2.999999999999927613 ) ) ;
#10171 = ORIENTED_EDGE ( 'NONE', *, *, #1216, .F. ) ;
#10172 = EDGE_CURVE ( 'NONE', #346, #2046, #4113, .T. ) ;
#10173 = ORIENTED_EDGE ( 'NONE', *, *, #268, .F. ) ;
#10174 = DIRECTION ( 'NONE',  ( 0.000000000000000000, 0.000000000000000000, 1.000000000000000000 ) ) ;
#10175 = EDGE_CURVE ( 'NONE', #3126, #10414, #8630, .T. ) ;
#10176 = CARTESIAN_POINT ( 'NONE',  ( -10.19839929293507552, 3.081249999044084475, 24.62111388749999463 ) ) ;
#10177 = CARTESIAN_POINT ( 'NONE',  ( 19.74999999999998934, 25.00000000000000000, -3.000000000000067946 ) ) ;
#10178 = CARTESIAN_POINT ( 'NONE',  ( -10.19839929293505776, 0.7062499990440844755, -24.62111388750000174 ) ) ;
#10179 = CARTESIAN_POINT ( 'NONE',  ( -17.40975659021752975, 2.593749999044084653, -17.40975659021752975 ) ) ;
#10180 = CARTESIAN_POINT ( 'NONE',  ( -12.47307621135344391, -0.001000000000001000089, -15.60400172474256131 ) ) ;
#10181 = EDGE_CURVE ( 'NONE', #4628, #2787, #1079, .T. ) ;
#10182 = EDGE_LOOP ( 'NONE', ( #4223, #586, #8331, #1596, #9357, #1017 ) ) ;
#10183 = CARTESIAN_POINT ( 'NONE',  ( 12.47307621135333200, 28.00000000000000000, 15.60400172474264835 ) ) ;
#10184 = LINE ( 'NONE', #10132, #6184 ) ;
#10185 = LINE ( 'NONE', #1970, #4970 ) ;
#10186 = COLOUR_RGB ( '', 0.66274510, 0.83137255, 0.94901961) ;
#10187 = CARTESIAN_POINT ( 'NONE',  ( -17.40975659021753330, 4.843749999044083765, 17.40975659021752975 ) ) ;
#10188 = FACE_OUTER_BOUND ( 'NONE', #3594, .T. ) ;
#10189 = VERTEX_POINT ( 'NONE', #4455 ) ;
#10190 = ORIENTED_EDGE ( 'NONE', *, *, #5575, .T. ) ;
#10191 = CARTESIAN_POINT ( 'NONE',  ( 2.449293598294706414E-16, 25.00000000000000355, 2.000000000000000000 ) ) ;
#10192 = STYLED_ITEM ( 'NONE', ( #1527 ), #10510 ) ;
#10193 = EDGE_CURVE ( 'NONE', #7302, #4608, #246, .T. ) ;
#10194 = AXIS2_PLACEMENT_3D ( 'NONE', #1115, #3643, #9584 ) ;
#10195 = DIRECTION ( 'NONE',  ( 0.000000000000000000, 1.000000000000000000, 0.000000000000000000 ) ) ;
#10196 = CARTESIAN_POINT ( 'NONE',  ( 25.00000000000000000, 2.062500000000000000, -10.35533905932737753 ) ) ;
#10197 = CARTESIAN_POINT ( 'NONE',  ( 6.999999999999997335, 20.00000000000000355, 2.444036937190192402E-14 ) ) ;
#10198 = DIRECTION ( 'NONE',  ( -0.000000000000000000, -0.000000000000000000, 1.000000000000000000 ) ) ;
#10199 = DIRECTION ( 'NONE',  ( 0.000000000000000000, -0.000000000000000000, 1.000000000000000000 ) ) ;
#10200 = CARTESIAN_POINT ( 'NONE',  ( 20.96888409245972440, 4.999999999999998224, 13.39592759827673518 ) ) ;
#10201 = AXIS2_PLACEMENT_3D ( 'NONE', #1850, #3490, #5233 ) ;
#10202 = AXIS2_PLACEMENT_3D ( 'NONE', #9461, #8447, #5273 ) ;
#10203 = ORIENTED_EDGE ( 'NONE', *, *, #2722, .F. ) ;
#10204 = LINE ( 'NONE', #2619, #4583 ) ;
#10205 = PRESENTATION_STYLE_ASSIGNMENT (( #5079 ) ) ;
#10206 = ADVANCED_BREP_SHAPE_REPRESENTATION ( '', ( #7050, #7040 ), #1019 ) ;
#10207 = FACE_OUTER_BOUND ( 'NONE', #7993, .T. ) ;
#10208 = CYLINDRICAL_SURFACE ( 'NONE', #9903, 2.999999999999999112 ) ;
#10209 = CARTESIAN_POINT ( 'NONE',  ( 0.000000000000000000, 5.000000000000000000, 0.000000000000000000 ) ) ;
#10210 = FACE_OUTER_BOUND ( 'NONE', #1392, .T. ) ;
#10211 = DIRECTION ( 'NONE',  ( 0.000000000000000000, 0.000000000000000000, 1.000000000000000000 ) ) ;
#10212 = CYLINDRICAL_SURFACE ( 'NONE', #497, 25.00000000000000000 ) ;
#10213 = CARTESIAN_POINT ( 'NONE',  ( 1.507608415688466075E-15, 1.643749999044084475, -24.62111388750000174 ) ) ;
#10214 = LINE ( 'NONE', #5859, #190 ) ;
#10215 = CARTESIAN_POINT ( 'NONE',  ( -17.67766952966369232, 1.237499998088169129, 17.67766952966368876 ) ) ;
#10216 = CARTESIAN_POINT ( 'NONE',  ( -5.000000000000000000, 0.000000000000000000, 0.000000000000000000 ) ) ;
#10217 = VERTEX_POINT ( 'NONE', #1787 ) ;
#10218 = DIRECTION ( 'NONE',  ( 1.000000000000000000, 0.000000000000000000, 0.000000000000000000 ) ) ;
#10219 = CARTESIAN_POINT ( 'NONE',  ( -17.67766952966368876, 0.9874999980881691286, -17.67766952966369232 ) ) ;
#10220 = SURFACE_SIDE_STYLE ('',( #10342 ) ) ;
#10221 = PLANE ( 'NONE',  #5369 ) ;
#10222 = FACE_BOUND ( 'NONE', #2816, .T. ) ;
#10223 = EDGE_CURVE ( 'NONE', #2972, #5481, #905, .T. ) ;
#10224 = CARTESIAN_POINT ( 'NONE',  ( -10.35533905932739174, 2.299999998088168685, 24.99999999999999289 ) ) ;
#10225 = CARTESIAN_POINT ( 'NONE',  ( 82.32050807568876394, 92.28203230275514102, 0.000000000000000000 ) ) ;
#10226 = CARTESIAN_POINT ( 'NONE',  ( -25.00000000000000000, 4.500000000000000888, -3.061616997868383043E-15 ) ) ;
#10227 = CIRCLE ( 'NONE', #9886, 6.000000000000000888 ) ;
#10228 = VECTOR ( 'NONE', #5925, 1000.000000000000114 ) ;
#10229 = VERTEX_POINT ( 'NONE', #10403 ) ;
#10230 = EDGE_LOOP ( 'NONE', ( #4202, #5687, #3260, #1566 ) ) ;
#10231 = ORIENTED_EDGE ( 'NONE', *, *, #7258, .T. ) ;
#10232 = EDGE_CURVE ( 'NONE', #2102, #4070, #4859, .T. ) ;
#10233 = CARTESIAN_POINT ( 'NONE',  ( 9.875000000000023093, 25.00000000000000000, 17.10400172474264835 ) ) ;
#10234 = CARTESIAN_POINT ( 'NONE',  ( -17.40975659021753330, 0.8437499990440846531, 17.40975659021752975 ) ) ;
#10235 = CARTESIAN_POINT ( 'NONE',  ( 1.530808498934191521E-15, 0.8624999980881691286, -25.00000000000000000 ) ) ;
#10236 = CARTESIAN_POINT ( 'NONE',  ( 10.35533905932738286, 4.424999998088169129, 24.99999999999999645 ) ) ;
#10237 = CARTESIAN_POINT ( 'NONE',  ( -17.40975659021752975, 4.593749999044084653, -17.40975659021752975 ) ) ;
#10238 = CARTESIAN_POINT ( 'NONE',  ( -25.00000000000000000, 3.049999998088169129, -10.35533905932738108 ) ) ;
#10239 = CIRCLE ( 'NONE', #3526, 25.00000000000000000 ) ;
#10240 = EDGE_CURVE ( 'NONE', #3898, #1513, #6820, .T. ) ;
#10241 = CARTESIAN_POINT ( 'NONE',  ( -1.500000000000001332, -1.935951399190116865E-16, -6.975000000000008527 ) ) ;
#10242 = EDGE_CURVE ( 'NONE', #4148, #2830, #5877, .T. ) ;
#10243 = FACE_OUTER_BOUND ( 'NONE', #2771, .T. ) ;
#10244 = CARTESIAN_POINT ( 'NONE',  ( -7.276923788646446845, 28.00000000000000000, 18.60400172474275848 ) ) ;
#10245 = LINE ( 'NONE', #8529, #9591 ) ;
#10246 = ORIENTED_EDGE ( 'NONE', *, *, #204, .F. ) ;
#10247 = EDGE_LOOP ( 'NONE', ( #9463, #9104, #7183, #6704, #9425 ) ) ;
#10248 = VERTEX_POINT ( 'NONE', #2595 ) ;
#10249 = ADVANCED_FACE ( 'NONE', ( #9283 ), #6345, .F. ) ;
#10250 = VECTOR ( 'NONE', #4160, 1000.000000000000000 ) ;
#10251 = STYLED_ITEM ( 'NONE', ( #10205 ), #3457 ) ;
#10252 = ORIENTED_EDGE ( 'NONE', *, *, #8344, .T. ) ;
#10253 = CARTESIAN_POINT ( 'NONE',  ( -1.500000000000001332, 0.000000000000000000, 0.000000000000000000 ) ) ;
#10254 = DIRECTION ( 'NONE',  ( 0.000000000000000000, -0.000000000000000000, 1.000000000000000000 ) ) ;
#10255 = DIRECTION ( 'NONE',  ( 1.000000000000000000, 0.000000000000000000, 0.000000000000000000 ) ) ;
#10256 = PLANE ( 'NONE',  #6573 ) ;
#10257 = LINE ( 'NONE', #10084, #49 ) ;
#10258 = DIRECTION ( 'NONE',  ( -0.7071067811865457964, 8.659560562354953812E-17, -0.7071067811865492381 ) ) ;
#10259 = CARTESIAN_POINT ( 'NONE',  ( -25.00000000000000000, 1.437500000000000000, -10.35533905932738108 ) ) ;
#10260 = CARTESIAN_POINT ( 'NONE',  ( 17.40975659021752975, 4.518749999044084475, -17.40975659021752975 ) ) ;
#10261 = AXIS2_PLACEMENT_3D ( 'NONE', #5236, #9531, #2716 ) ;
#10262 = ADVANCED_FACE ( 'NONE', ( #8618 ), #2634, .F. ) ;
#10263 = VERTEX_POINT ( 'NONE', #7798 ) ;
#10264 = DIRECTION ( 'NONE',  ( 0.000000000000000000, 1.000000000000000000, 0.000000000000000000 ) ) ;
#10265 = CARTESIAN_POINT ( 'NONE',  ( -17.67766952966368876, 4.987499998088170017, -17.67766952966369232 ) ) ;
#10266 =( NAMED_UNIT ( * ) SI_UNIT ( $, .STERADIAN. ) SOLID_ANGLE_UNIT ( ) );
#10267 = CARTESIAN_POINT ( 'NONE',  ( -24.62111388750000884, 4.945761085427167636, 8.486877225504324329 ) ) ;
#10268 = DIRECTION ( 'NONE',  ( 0.000000000000000000, -0.000000000000000000, -1.000000000000000000 ) ) ;
#10269 = SHAPE_DEFINITION_REPRESENTATION ( #6891, #5436 ) ;
#10270 = DIRECTION ( 'NONE',  ( 0.2499999999999980016, -0.8660254037844380415, 0.4330127018922217408 ) ) ;
#10271 =( BOUNDED_CURVE ( )  B_SPLINE_CURVE ( 3, ( #10314, #5296, #1248, #5557 ),
 .UNSPECIFIED., .F., .F. ) 
 B_SPLINE_CURVE_WITH_KNOTS ( ( 4, 4 ),
 ( 2.284520705739661484, 2.356010155625181568 ),
 .UNSPECIFIED. ) 
 CURVE ( )  GEOMETRIC_REPRESENTATION_ITEM ( )  RATIONAL_B_SPLINE_CURVE ( ( 1.000000000000000000, 0.9995741502243209453, 0.9995741502243209453, 1.000000000000000000 ) ) 
 REPRESENTATION_ITEM ( '' )  );
#10272 = CARTESIAN_POINT ( 'NONE',  ( 0.000000000000000000, 10.00000000000000355, 0.000000000000000000 ) ) ;
#10273 = CARTESIAN_POINT ( 'NONE',  ( 17.40975659021752620, 5.093749999044084653, 17.40975659021753330 ) ) ;
#10274 = VECTOR ( 'NONE', #1775, 1000.000000000000000 ) ;
#10275 = ADVANCED_FACE ( 'NONE', ( #7679 ), #4319, .T. ) ;
#10276 = AXIS2_PLACEMENT_3D ( 'NONE', #10699, #2137, #5515 ) ;
#10277 = CARTESIAN_POINT ( 'NONE',  ( 17.40975659021752620, 1.268749999044084698, 17.40975659021753330 ) ) ;
#10278 = VECTOR ( 'NONE', #6929, 1000.000000000000114 ) ;
#10279 = CARTESIAN_POINT ( 'NONE',  ( 10.19839929293505953, 3.581249999044085364, -24.62111388750000174 ) ) ;
#10280 = CARTESIAN_POINT ( 'NONE',  ( -5.796693311223863887, 10.00000000000000355, -3.924072712834521415 ) ) ;
#10281 = CARTESIAN_POINT ( 'NONE',  ( 24.62111388749999463, 4.156249999044083765, 10.19839929293507730 ) ) ;
#10282 = CARTESIAN_POINT ( 'NONE',  ( -10.19839929293505776, 1.706249999044084698, -24.62111388750000174 ) ) ;
#10283 = ORIENTED_EDGE ( 'NONE', *, *, #8396, .T. ) ;
#10284 = PLANE ( 'NONE',  #7940 ) ;
#10285 = DIRECTION ( 'NONE',  ( 1.000000000000000000, 0.000000000000000000, 0.000000000000000000 ) ) ;
#10286 = CARTESIAN_POINT ( 'NONE',  ( 25.00000000000000000, 1.612499998088169351, 0.000000000000000000 ) ) ;
#10287 = VECTOR ( 'NONE', #1310, 1000.000000000000000 ) ;
#10288 = FACE_BOUND ( 'NONE', #6549, .T. ) ;
#10289 = CARTESIAN_POINT ( 'NONE',  ( 3.433012701892224516, 10.00000000000000355, -4.946152422706625806 ) ) ;
#10290 = DIRECTION ( 'NONE',  ( 0.000000000000000000, 1.000000000000000000, 0.000000000000000000 ) ) ;
#10291 = CARTESIAN_POINT ( 'NONE',  ( -4.592425496802574367E-15, 2.750000000000000000, 25.00000000000000000 ) ) ;
#10292 = CIRCLE ( 'NONE', #758, 12.77350269189627063 ) ;
#10293 = AXIS2_PLACEMENT_3D ( 'NONE', #10272, #2744, #10211 ) ;
#10294 = ORIENTED_EDGE ( 'NONE', *, *, #2650, .F. ) ;
#10295 = ORIENTED_EDGE ( 'NONE', *, *, #7682, .F. ) ;
#10296 = AXIS2_PLACEMENT_3D ( 'NONE', #7673, #8434, #5792 ) ;
#10297 = CARTESIAN_POINT ( 'NONE',  ( 1.507608415688466075E-15, 4.643749999044085364, -24.62111388750000174 ) ) ;
#10298 = CARTESIAN_POINT ( 'NONE',  ( -10.19839929293507552, 1.081249999044084475, 24.62111388749999463 ) ) ;
#10299 = CARTESIAN_POINT ( 'NONE',  ( -25.00000000000000000, 4.049999998088169129, -10.35533905932738108 ) ) ;
#10300 = AXIS2_PLACEMENT_3D ( 'NONE', #1215, #1170, #2741 ) ;
#10301 = CARTESIAN_POINT ( 'NONE',  ( 10.19839929293506486, 3.031249999044084653, 24.62111388749999819 ) ) ;
#10302 = CIRCLE ( 'NONE', #759, 30.00000000000000000 ) ;
#10303 = CARTESIAN_POINT ( 'NONE',  ( 0.000000000000000000, -1.000000000000003331, 0.5773502691896272854 ) ) ;
#10304 = DIRECTION ( 'NONE',  ( 0.4330127018922172999, 0.8660254037844380415, 0.2500000000000055511 ) ) ;
#10305 = CARTESIAN_POINT ( 'NONE',  ( 24.81055694375000087, 0.1093749995220422710, 0.000000000000000000 ) ) ;
#10306 = DIRECTION ( 'NONE',  ( -0.000000000000000000, -1.000000000000000000, -0.000000000000000000 ) ) ;
#10307 = CONICAL_SURFACE ( 'NONE', #5720, 4.000000000000006217, 0.1745329251994333364 ) ;
#10308 = CARTESIAN_POINT ( 'NONE',  ( -10.35533905932739174, 0.6875000000000000000, 24.99999999999999289 ) ) ;
#10309 = DIRECTION ( 'NONE',  ( 0.000000000000000000, -1.000000000000000000, 0.000000000000000000 ) ) ;
#10310 = ORIENTED_EDGE ( 'NONE', *, *, #7007, .F. ) ;
#10311 = ORIENTED_EDGE ( 'NONE', *, *, #5552, .F. ) ;
#10312 = VERTEX_POINT ( 'NONE', #4504 ) ;
#10313 = EDGE_CURVE ( 'NONE', #1642, #9966, #1062, .T. ) ;
#10314 = CARTESIAN_POINT ( 'NONE',  ( -3.500000000000049294, 20.00000000000000355, 6.062177826491040200 ) ) ;
#10315 = CARTESIAN_POINT ( 'NONE',  ( -3.000000000000000888, -0.001000000000001000089, -15.75000000000000355 ) ) ;
#10316 = VERTEX_POINT ( 'NONE', #9390 ) ;
#10317 = CARTESIAN_POINT ( 'NONE',  ( 0.000000000000000000, 5.000000000000000000, 0.000000000000000000 ) ) ;
#10318 = EDGE_CURVE ( 'NONE', #39, #6463, #8588, .T. ) ;
#10319 = DIRECTION ( 'NONE',  ( 0.000000000000000000, 0.000000000000000000, 1.000000000000000000 ) ) ;
#10320 = FACE_OUTER_BOUND ( 'NONE', #777, .T. ) ;
#10321 = CARTESIAN_POINT ( 'NONE',  ( -7.276923788646447733, 25.00000000000000000, 18.60400172474275848 ) ) ;
#10322 = CARTESIAN_POINT ( 'NONE',  ( 0.000000000000000000, 10.00000000000000355, 0.000000000000000000 ) ) ;
#10323 = CARTESIAN_POINT ( 'NONE',  ( -4.522825247065398226E-15, 5.143749999044084475, 24.62111388750000174 ) ) ;
#10324 = EDGE_CURVE ( 'NONE', #3699, #3734, #4258, .T. ) ;
#10325 = VERTEX_POINT ( 'NONE', #3413 ) ;
#10326 = PRODUCT_DEFINITION_SHAPE ( 'NONE', 'NONE',  #10952 ) ;
#10327 = CARTESIAN_POINT ( 'NONE',  ( -18.60400172474273717, 28.00000000000000000, -7.276923788646511682 ) ) ;
#10328 = CARTESIAN_POINT ( 'NONE',  ( 17.40975659021752620, 2.268749999044084475, 17.40975659021753330 ) ) ;
#10329 = DIRECTION ( 'NONE',  ( 0.000000000000000000, 0.000000000000000000, 1.000000000000000000 ) ) ;
#10330 = CONTEXT_DEPENDENT_SHAPE_REPRESENTATION ( #9712, #1246 ) ;
#10331 = EDGE_CURVE ( 'NONE', #9729, #457, #9300, .T. ) ;
#10332 = CARTESIAN_POINT ( 'NONE',  ( 6.123233995736763324E-16, 88.00000000000001421, 4.999999999999997335 ) ) ;
#10333 = CARTESIAN_POINT ( 'NONE',  ( 3.418204983771598122E-15, -58.00000000000000000, -27.91176187412963117 ) ) ;
#10334 = CARTESIAN_POINT ( 'NONE',  ( -17.40975659021752975, 4.593749999044084653, -17.40975659021752975 ) ) ;
#10335 = CARTESIAN_POINT ( 'NONE',  ( -17.40975659021753330, 1.018749999044084698, 17.40975659021752975 ) ) ;
#10336 = DIRECTION ( 'NONE',  ( 0.000000000000000000, 0.000000000000000000, 1.000000000000000000 ) ) ;
#10337 = DIRECTION ( 'NONE',  ( 0.000000000000000000, 1.000000000000000000, 0.000000000000000000 ) ) ;
#10338 = CARTESIAN_POINT ( 'NONE',  ( -17.67766952966368876, 0.9874999980881691286, -17.67766952966369232 ) ) ;
#10339 = DIRECTION ( 'NONE',  ( 0.5000000000000009992, -0.8660254037844380415, 1.745740669421570228E-15 ) ) ;
#10340 = ORIENTED_EDGE ( 'NONE', *, *, #7663, .T. ) ;
#10341 = DIRECTION ( 'NONE',  ( -1.000000000000000000, 0.000000000000000000, 0.000000000000000000 ) ) ;
#10342 = SURFACE_STYLE_FILL_AREA ( #893 ) ;
#10343 = CARTESIAN_POINT ( 'NONE',  ( -4.592425496802574367E-15, 4.750000000000000000, 25.00000000000000000 ) ) ;
#10344 = CARTESIAN_POINT ( 'NONE',  ( -1.400000000000001910, 7.511012776518211958E-16, 5.000000000000000000 ) ) ;
#10345 = CARTESIAN_POINT ( 'NONE',  ( -10.35533905932739174, 2.299999998088169129, 24.99999999999999289 ) ) ;
#10346 = ORIENTED_EDGE ( 'NONE', *, *, #9998, .F. ) ;
#10347 = CARTESIAN_POINT ( 'NONE',  ( 1.500000000000001332, 1.119140903701213403E-15, 7.399999999999999467 ) ) ;
#10348 = CARTESIAN_POINT ( 'NONE',  ( 24.62111388749999463, 5.331249999044085364, 10.19839929293507730 ) ) ;
#10349 = CARTESIAN_POINT ( 'NONE',  ( 5.796693311223892309, 10.00000000000000355, 3.924072712834481447 ) ) ;
#10350 = CARTESIAN_POINT ( 'NONE',  ( -10.35533905932739174, 2.299999998088168685, 24.99999999999999289 ) ) ;
#10351 = CARTESIAN_POINT ( 'NONE',  ( -24.62111388750000174, 3.656249999044084653, -10.19839929293506131 ) ) ;
#10352 = DIRECTION ( 'NONE',  ( 0.000000000000000000, 0.000000000000000000, 1.000000000000000000 ) ) ;
#10353 = DIRECTION ( 'NONE',  ( -0.000000000000000000, -1.000000000000000000, -0.000000000000000000 ) ) ;
#10354 = FACE_BOUND ( 'NONE', #607, .T. ) ;
#10355 = DIRECTION ( 'NONE',  ( 0.000000000000000000, 0.000000000000000000, 1.000000000000000000 ) ) ;
#10356 = CARTESIAN_POINT ( 'NONE',  ( -3.924072712834500543, 10.00000000000000355, 5.796693311223878098 ) ) ;
#10357 = CARTESIAN_POINT ( 'NONE',  ( -2.262820851736579986, 10.00000000000000355, 9.633606397919624698 ) ) ;
#10358 = ORIENTED_EDGE ( 'NONE', *, *, #5846, .T. ) ;
#10359 = VERTEX_POINT ( 'NONE', #6031 ) ;
#10360 = EDGE_LOOP ( 'NONE', ( #9536, #2056, #4067, #5642, #6060 ) ) ;
#10361 = PLANE ( 'NONE',  #8235 ) ;
#10362 = STYLED_ITEM ( 'NONE', ( #5219 ), #5075 ) ;
#10363 = DIRECTION ( 'NONE',  ( 0.8660254037844362651, 0.000000000000000000, -0.5000000000000041078 ) ) ;
#10364 = VERTEX_POINT ( 'NONE', #10163 ) ;
#10365 = DIRECTION ( 'NONE',  ( 0.000000000000000000, -2.775557561562888270E-17, -1.000000000000000000 ) ) ;
#10366 = FACE_OUTER_BOUND ( 'NONE', #6140, .T. ) ;
#10367 =( BOUNDED_CURVE ( )  B_SPLINE_CURVE ( 2, ( #3012, #7031, #2860, #6205, #9563, #5380, #6258, #5468, #8835 ),
 .UNSPECIFIED., .F., .F. ) 
 B_SPLINE_CURVE_WITH_KNOTS ( ( 3, 2, 2, 2, 3 ),
 ( 0.05000000000000000278, 0.07500000000000001110, 0.1000000000000000194, 0.1250000000000000278, 0.1500000000000000222 ),
 .UNSPECIFIED. ) 
 CURVE ( )  GEOMETRIC_REPRESENTATION_ITEM ( )  RATIONAL_B_SPLINE_CURVE ( ( 1.000000000000000000, 0.9238795325112867385, 1.000000000000000000, 0.9238795325112867385, 1.000000000000000000, 0.9238795325112867385, 1.000000000000000000, 0.9238795325112866275, 1.000000000000000000 ) ) 
 REPRESENTATION_ITEM ( '' )  );
#10368 = DIRECTION ( 'NONE',  ( 0.000000000000000000, 0.000000000000000000, 1.000000000000000000 ) ) ;
#10369 = EDGE_CURVE ( 'NONE', #5054, #2200, #2164, .T. ) ;
#10370 = DIRECTION ( 'NONE',  ( 0.000000000000000000, 1.000000000000000000, 0.000000000000000000 ) ) ;
#10371 = DIRECTION ( 'NONE',  ( 0.000000000000000000, 0.000000000000000000, -1.000000000000000000 ) ) ;
#10372 = CARTESIAN_POINT ( 'NONE',  ( -24.62111388750000884, 3.956249999044084920, 10.19839929293505421 ) ) ;
#10373 = VERTEX_POINT ( 'NONE', #1324 ) ;
#10374 = ORIENTED_EDGE ( 'NONE', *, *, #204, .T. ) ;
#10375 = CIRCLE ( 'NONE', #6314, 12.77350269189627063 ) ;
#10376 = ADVANCED_FACE ( 'NONE', ( #4605 ), #8890, .T. ) ;
#10377 = EDGE_LOOP ( 'NONE', ( #4578, #8977, #8035, #65 ) ) ;
#10378 = CARTESIAN_POINT ( 'NONE',  ( -17.10400172474275848, 25.00000000000000000, -9.874999999999836575 ) ) ;
#10379 = CARTESIAN_POINT ( 'NONE',  ( 15.60400172474260927, 25.00000000000000000, -12.47307621135339062 ) ) ;
#10380 = CARTESIAN_POINT ( 'NONE',  ( 24.62111388749999108, 1.331249999044084475, 10.19839929293507730 ) ) ;
#10381 = VERTEX_POINT ( 'NONE', #386 ) ;
#10382 = DIRECTION ( 'NONE',  ( -0.000000000000000000, -1.000000000000000000, -0.000000000000000000 ) ) ;
#10383 = CARTESIAN_POINT ( 'NONE',  ( 13.63990010960492860, -0.001000000000001000089, 7.874999999999965361 ) ) ;
#10384 = CIRCLE ( 'NONE', #1218, 0.7499999999999997780 ) ;
#10385 = DIRECTION ( 'NONE',  ( 0.000000000000000000, 0.000000000000000000, 1.000000000000000000 ) ) ;
#10386 = EDGE_CURVE ( 'NONE', #5893, #7313, #8783, .T. ) ;
#10387 = VECTOR ( 'NONE', #5146, 1000.000000000000000 ) ;
#10388 = EDGE_CURVE ( 'NONE', #2980, #5115, #7191, .T. ) ;
#10389 = CARTESIAN_POINT ( 'NONE',  ( 1.530808498934191521E-15, 2.250000000000000444, -25.00000000000000000 ) ) ;
#10390 = CIRCLE ( 'NONE', #10202, 12.77350269189627063 ) ;
#10391 = CYLINDRICAL_SURFACE ( 'NONE', #7910, 2.999999999999997335 ) ;
#10392 = CARTESIAN_POINT ( 'NONE',  ( 17.40975659021752620, 1.268749999044084475, 17.40975659021753330 ) ) ;
#10393 = ORIENTED_EDGE ( 'NONE', *, *, #9160, .F. ) ;
#10394 = CARTESIAN_POINT ( 'NONE',  ( 3.061616997868383043E-15, 20.00000000000000355, 25.00000000000000000 ) ) ;
#10395 = CARTESIAN_POINT ( 'NONE',  ( 0.000000000000000000, 20.00000000000000355, -25.00000000000000000 ) ) ;
#10396 = CARTESIAN_POINT ( 'NONE',  ( -4.522825247065398226E-15, 0.9687499990440845421, 24.62111388750000174 ) ) ;
#10397 = LINE ( 'NONE', #2011, #5775 ) ;
#10398 = VERTEX_POINT ( 'NONE', #441 ) ;
#10399 = ADVANCED_FACE ( 'NONE', ( #6303 ), #10391, .F. ) ;
#10400 = ORIENTED_EDGE ( 'NONE', *, *, #9143, .F. ) ;
#10401 = PRODUCT_DEFINITION_FORMATION_WITH_SPECIFIED_SOURCE ( 'ANY', '', #6284, .NOT_KNOWN. ) ;
#10402 = CARTESIAN_POINT ( 'NONE',  ( 17.40975659021752620, 2.093749999044084653, 17.40975659021753330 ) ) ;
#10403 = CARTESIAN_POINT ( 'NONE',  ( -6.999999999999997335, 20.00000000000000355, -7.332110811570577522E-14 ) ) ;
#10404 = CARTESIAN_POINT ( 'NONE',  ( -4.592425496802574367E-15, 3.362499998088169129, 25.00000000000000000 ) ) ;
#10405 = CARTESIAN_POINT ( 'NONE',  ( 25.00000000000000000, 5.000000000000000000, 0.000000000000000000 ) ) ;
#10406 = DIRECTION ( 'NONE',  ( 0.000000000000000000, 1.000000000000000000, 0.000000000000000000 ) ) ;
#10407 = CARTESIAN_POINT ( 'NONE',  ( -5.796693311223946488, 19.03096903053430466, 3.924072712834398846 ) ) ;
#10408 = CARTESIAN_POINT ( 'NONE',  ( -25.00000000000000000, 2.500000000000000000, -3.061616997868383043E-15 ) ) ;
#10409 = FACE_OUTER_BOUND ( 'NONE', #2677, .T. ) ;
#10410 = CIRCLE ( 'NONE', #6356, 2.999999999999997335 ) ;
#10411 = AXIS2_PLACEMENT_3D ( 'NONE', #2929, #3832, #560 ) ;
#10412 = DIRECTION ( 'NONE',  ( -1.000000000000000000, 0.000000000000000000, 0.000000000000000000 ) ) ;
#10413 = VERTEX_POINT ( 'NONE', #4657 ) ;
#10414 = VERTEX_POINT ( 'NONE', #5578 ) ;
#10415 = EDGE_LOOP ( 'NONE', ( #10455, #4515, #3000 ) ) ;
#10416 = PRODUCT_DEFINITION_SHAPE ( 'NONE', 'NONE',  #7512 ) ;
#10417 = AXIS2_PLACEMENT_3D ( 'NONE', #10209, #5140, #10152 ) ;
#10418 = VECTOR ( 'NONE', #6435, 1000.000000000000114 ) ;
#10419 = DIRECTION ( 'NONE',  ( -0.8660254037844431485, 0.000000000000000000, -0.4999999999999920064 ) ) ;
#10420 = FACE_OUTER_BOUND ( 'NONE', #1577, .T. ) ;
#10421 = DIRECTION ( 'NONE',  ( 0.000000000000000000, 0.000000000000000000, 1.000000000000000000 ) ) ;
#10422 = DIRECTION ( 'NONE',  ( 0.000000000000000000, 0.000000000000000000, -1.000000000000000000 ) ) ;
#10423 = CARTESIAN_POINT ( 'NONE',  ( 0.000000000000000000, 10.00000000000000355, 0.000000000000000000 ) ) ;
#10424 = CARTESIAN_POINT ( 'NONE',  ( -17.67766952966369232, 1.625000000000000222, 17.67766952966368876 ) ) ;
#10425 = CARTESIAN_POINT ( 'NONE',  ( -4.522825247065398226E-15, 4.143749999044083587, 24.62111388750000174 ) ) ;
#10426 = CIRCLE ( 'NONE', #8471, 6.975000000000008527 ) ;
#10427 =( GEOMETRIC_REPRESENTATION_CONTEXT ( 3 ) GLOBAL_UNCERTAINTY_ASSIGNED_CONTEXT ( ( #3041 ) ) GLOBAL_UNIT_ASSIGNED_CONTEXT ( ( #5577, #599, #7278 ) ) REPRESENTATION_CONTEXT ( 'NONE', 'WORKASPACE' ) );
#10428 = ORIENTED_EDGE ( 'NONE', *, *, #2792, .T. ) ;
#10429 = VERTEX_POINT ( 'NONE', #490 ) ;
#10430 = EDGE_CURVE ( 'NONE', #3638, #5087, #8782, .T. ) ;
#10431 = AXIS2_PLACEMENT_3D ( 'NONE', #6534, #413, #9015 ) ;
#10432 = AXIS2_PLACEMENT_3D ( 'NONE', #1505, #4115, #6600 ) ;
#10433 = CARTESIAN_POINT ( 'NONE',  ( -24.62111388750000174, 1.831249999044084475, -10.19839929293506131 ) ) ;
#10434 =( BOUNDED_CURVE ( )  B_SPLINE_CURVE ( 3, ( #3879, #6479, #557, #9784 ),
 .UNSPECIFIED., .F., .F. ) 
 B_SPLINE_CURVE_WITH_KNOTS ( ( 4, 4 ),
 ( 3.927175151554403332, 3.998664601439923860 ),
 .UNSPECIFIED. ) 
 CURVE ( )  GEOMETRIC_REPRESENTATION_ITEM ( )  RATIONAL_B_SPLINE_CURVE ( ( 1.000000000000000000, 0.9995741502243209453, 0.9995741502243209453, 1.000000000000000000 ) ) 
 REPRESENTATION_ITEM ( '' )  );
#10435 = DIRECTION ( 'NONE',  ( 0.000000000000000000, 0.000000000000000000, 1.000000000000000000 ) ) ;
#10436 = DIRECTION ( 'NONE',  ( -1.734723475976808672E-15, 0.000000000000000000, 1.000000000000000000 ) ) ;
#10437 = FACE_OUTER_BOUND ( 'NONE', #7549, .T. ) ;
#10438 = EDGE_CURVE ( 'NONE', #5323, #6538, #10529, .T. ) ;
#10439 = ORIENTED_EDGE ( 'NONE', *, *, #3062, .F. ) ;
#10440 = AXIS2_PLACEMENT_3D ( 'NONE', #5500, #9649, #4007 ) ;
#10441 = EDGE_CURVE ( 'NONE', #10864, #3965, #8418, .T. ) ;
#10442 = ADVANCED_FACE ( 'NONE', ( #3862 ), #9618, .T. ) ;
#10443 = CARTESIAN_POINT ( 'NONE',  ( -10.19839929293507552, 5.081249999044084475, 24.62111388749999463 ) ) ;
#10444 = DIRECTION ( 'NONE',  ( 0.000000000000000000, 0.000000000000000000, 1.000000000000000000 ) ) ;
#10445 = CARTESIAN_POINT ( 'NONE',  ( -24.82160728492508639, 5.000000000000000888, 0.8552643272782575190 ) ) ;
#10446 = CARTESIAN_POINT ( 'NONE',  ( -1.500000000000000444, 83.00000000000000000, -1.500000000000000222 ) ) ;
#10447 = ORIENTED_EDGE ( 'NONE', *, *, #916, .T. ) ;
#10448 = FACE_OUTER_BOUND ( 'NONE', #1032, .T. ) ;
#10449 = CARTESIAN_POINT ( 'NONE',  ( 11.06217782649109260, 10.00000000000000355, -6.386751345948115777 ) ) ;
#10450 = CARTESIAN_POINT ( 'NONE',  ( 1.507608415688466075E-15, 3.468749999044085097, -24.62111388750000174 ) ) ;
#10451 = CARTESIAN_POINT ( 'NONE',  ( 25.00000000000000000, 0.06249999999999997224, -10.35533905932737753 ) ) ;
#10452 = EDGE_CURVE ( 'NONE', #1429, #6472, #10367, .T. ) ;
#10453 = EDGE_LOOP ( 'NONE', ( #9154, #3353, #8199, #2396 ) ) ;
#10454 = ORIENTED_EDGE ( 'NONE', *, *, #7389, .T. ) ;
#10455 = ORIENTED_EDGE ( 'NONE', *, *, #7319, .T. ) ;
#10456 = VECTOR ( 'NONE', #7280, 1000.000000000000000 ) ;
#10457 = ORIENTED_EDGE ( 'NONE', *, *, #6870, .F. ) ;
#10458 = EDGE_CURVE ( 'NONE', #4034, #9769, #9979, .T. ) ;
#10459 = CIRCLE ( 'NONE', #4284, 6.999999999999997335 ) ;
#10460 = DIRECTION ( 'NONE',  ( 0.000000000000000000, 0.000000000000000000, 1.000000000000000000 ) ) ;
#10461 = CARTESIAN_POINT ( 'NONE',  ( 10.19839929293505953, 2.406249999044085541, -24.62111388750000174 ) ) ;
#10462 = AXIS2_PLACEMENT_3D ( 'NONE', #8812, #7013, #10371 ) ;
#10463 = CARTESIAN_POINT ( 'NONE',  ( 10.19839929293506486, 1.206249999044084698, 24.62111388749999819 ) ) ;
#10464 = CARTESIAN_POINT ( 'NONE',  ( -25.00000000000001421, 2.562500000000000444, 10.35533905932737397 ) ) ;
#10465 = DIRECTION ( 'NONE',  ( 0.000000000000000000, -2.775557561562888270E-17, -1.000000000000000000 ) ) ;
#10466 = AXIS2_PLACEMENT_3D ( 'NONE', #431, #4799, #638 ) ;
#10467 = DIRECTION ( 'NONE',  ( 0.000000000000000000, 0.000000000000000000, 1.000000000000000000 ) ) ;
#10468 = DIRECTION ( 'NONE',  ( 0.000000000000000000, 1.000000000000000000, 0.000000000000000000 ) ) ;
#10469 = AXIS2_PLACEMENT_3D ( 'NONE', #10883, #3985, #9155 ) ;
#10470 = DIRECTION ( 'NONE',  ( 0.000000000000000000, -1.000000000000000000, 0.000000000000000000 ) ) ;
#10471 = EDGE_CURVE ( 'NONE', #4838, #2806, #9662, .T. ) ;
#10472 = AXIS2_PLACEMENT_3D ( 'NONE', #9477, #3671, #1152 ) ;
#10473 = EDGE_LOOP ( 'NONE', ( #3907, #10732, #6185, #679 ) ) ;
#10474 = ORIENTED_EDGE ( 'NONE', *, *, #8970, .T. ) ;
#10475 = AXIS2_PLACEMENT_3D ( 'NONE', #470, #3355, #4379 ) ;
#10476 = DIRECTION ( 'NONE',  ( 4.188538737677001009E-17, -0.9396926207859082059, 0.3420201433256694901 ) ) ;
#10477 = TOROIDAL_SURFACE ( 'NONE', #3391, 5.100000000000000533, 0.1000000000000001582 ) ;
#10478 = VECTOR ( 'NONE', #770, 1000.000000000000000 ) ;
#10479 = PLANE ( 'NONE',  #3942 ) ;
#10480 = CARTESIAN_POINT ( 'NONE',  ( 0.000000000000000000, 20.00000000000000355, 0.000000000000000000 ) ) ;
#10481 = CYLINDRICAL_SURFACE ( 'NONE', #1289, 27.91176187412963117 ) ;
#10482 = DIRECTION ( 'NONE',  ( 0.000000000000000000, 0.000000000000000000, -1.000000000000000000 ) ) ;
#10483 = DIRECTION ( 'NONE',  ( 0.6123724356957902515, 0.3535533905932737309, 0.7071067811865512365 ) ) ;
#10484 = VERTEX_POINT ( 'NONE', #5685 ) ;
#10485 = EDGE_LOOP ( 'NONE', ( #2221, #4719, #10792, #584 ) ) ;
#10486 = VECTOR ( 'NONE', #1692, 1000.000000000000000 ) ;
#10487 = ORIENTED_EDGE ( 'NONE', *, *, #7096, .F. ) ;
#10488 = CARTESIAN_POINT ( 'NONE',  ( -17.40975659021752975, 2.768749999044084475, -17.40975659021752975 ) ) ;
#10489 = CYLINDRICAL_SURFACE ( 'NONE', #700, 2.999999999999997335 ) ;
#10490 = PLANE ( 'NONE',  #7130 ) ;
#10491 = CARTESIAN_POINT ( 'NONE',  ( -17.10400172474254532, -0.001000000000001000089, 12.87500000000020073 ) ) ;
#10492 = LINE ( 'NONE', #7688, #2140 ) ;
#10493 = ORIENTED_EDGE ( 'NONE', *, *, #7804, .F. ) ;
#10494 = ORIENTED_EDGE ( 'NONE', *, *, #4669, .F. ) ;
#10495 =( BOUNDED_CURVE ( )  B_SPLINE_CURVE ( 2, ( #288, #3652, #235, #9516, #5326, #3596, #6984, #7035, #8016 ),
 .UNSPECIFIED., .F., .F. ) 
 B_SPLINE_CURVE_WITH_KNOTS ( ( 3, 2, 2, 2, 3 ),
 ( 0.4500000000000000111, 0.4749999999999999778, 0.5000000000000000000, 0.5250000000000000222, 0.5500000000000000444 ),
 .UNSPECIFIED. ) 
 CURVE ( )  GEOMETRIC_REPRESENTATION_ITEM ( )  RATIONAL_B_SPLINE_CURVE ( ( 1.000000000000000000, 0.9238795325112867385, 1.000000000000000000, 0.9238795325112867385, 1.000000000000000000, 0.9238795325112867385, 1.000000000000000000, 0.9238795325112867385, 1.000000000000000000 ) ) 
 REPRESENTATION_ITEM ( '' )  );
#10496 = CARTESIAN_POINT ( 'NONE',  ( 0.5590169943749494497, 0.000000000000000000, 0.000000000000000000 ) ) ;
#10497 = CARTESIAN_POINT ( 'NONE',  ( 1.530808498934191521E-15, 3.250000000000000444, -25.00000000000000000 ) ) ;
#10498 = CARTESIAN_POINT ( 'NONE',  ( -4.522825247065398226E-15, 1.143749999044084475, 24.62111388750000174 ) ) ;
#10499 = ORIENTED_EDGE ( 'NONE', *, *, #4030, .F. ) ;
#10500 = CARTESIAN_POINT ( 'NONE',  ( -20.63749999999999929, 7.511012776518219847E-16, 5.000000000000005329 ) ) ;
#10501 = CARTESIAN_POINT ( 'NONE',  ( 0.000000000000000000, -8.528980942125402365, 0.000000000000000000 ) ) ;
#10502 = ORIENTED_EDGE ( 'NONE', *, *, #478, .T. ) ;
#10503 = CARTESIAN_POINT ( 'NONE',  ( -17.40975659021753330, 3.843749999044085097, 17.40975659021752975 ) ) ;
#10504 = CARTESIAN_POINT ( 'NONE',  ( 25.00000000000000000, 2.674999998088169573, -10.35533905932737753 ) ) ;
#10505 = PRODUCT_DEFINITION_SHAPE ( 'NONE', 'NONE',  #10947 ) ;
#10506 = EDGE_CURVE ( 'NONE', #10548, #2423, #5738, .T. ) ;
#10507 = EDGE_CURVE ( 'NONE', #748, #9491, #2360, .T. ) ;
#10508 = ORIENTED_EDGE ( 'NONE', *, *, #6647, .T. ) ;
#10509 = ORIENTED_EDGE ( 'NONE', *, *, #3535, .T. ) ;
#10510 = MANIFOLD_SOLID_BREP ( 'OuterRace', #7722 ) ;
#10511 = ORIENTED_EDGE ( 'NONE', *, *, #2465, .T. ) ;
#10512 = EDGE_CURVE ( 'NONE', #1695, #8288, #1580, .T. ) ;
#10513 = CARTESIAN_POINT ( 'NONE',  ( -9.633606397919589170, 10.00000000000000355, -2.262820851736602190 ) ) ;
#10514 = CARTESIAN_POINT ( 'NONE',  ( -24.62111388750000174, 1.718749999044084431, -3.015216831376932151E-15 ) ) ;
#10515 = CARTESIAN_POINT ( 'NONE',  ( -24.62111388750000884, 2.956249999044084475, 10.19839929293505421 ) ) ;
#10516 = CARTESIAN_POINT ( 'NONE',  ( -10.35533905932737575, 1.312500000000000444, -25.00000000000000000 ) ) ;
#10517 = CARTESIAN_POINT ( 'NONE',  ( 6.566987298107765270, 19.74999999999999645, 0.5000000000000228706 ) ) ;
#10518 = CARTESIAN_POINT ( 'NONE',  ( 12.47307621135333200, 25.00000000000000000, 15.60400172474264835 ) ) ;
#10519 = CARTESIAN_POINT ( 'NONE',  ( 82.32050807568876394, 92.28203230275514102, -4.000000000000006217 ) ) ;
#10520 = CARTESIAN_POINT ( 'NONE',  ( 1.530808498934191521E-15, 3.862499998088169573, -25.00000000000000000 ) ) ;
#10521 = EDGE_CURVE ( 'NONE', #3614, #10892, #765, .T. ) ;
#10522 = VERTEX_POINT ( 'NONE', #4141 ) ;
#10523 = ORIENTED_EDGE ( 'NONE', *, *, #10104, .F. ) ;
#10524 = VERTEX_POINT ( 'NONE', #3223 ) ;
#10525 = EDGE_CURVE ( 'NONE', #4608, #3230, #7538, .T. ) ;
#10526 = CARTESIAN_POINT ( 'NONE',  ( 82.32050807568876394, 99.93473594742127375, 0.000000000000000000 ) ) ;
#10527 = DIRECTION ( 'NONE',  ( 0.000000000000000000, 0.000000000000000000, 1.000000000000000000 ) ) ;
#10528 = PLANE ( 'NONE',  #3005 ) ;
#10529 = B_SPLINE_CURVE_WITH_KNOTS ( 'NONE', 3,
 ( #1275, #338, #6359, #3704, #9667, #4553, #8737, #1224, #10445, #7859, #7961, #2004, #3808, #2093, #8053, #1176, #9718, #1369 ),
 .UNSPECIFIED., .F., .F.,
 ( 4, 2, 2, 2, 2, 2, 2, 2, 4 ),
 ( 0.000000000000000000, 0.004245714814779292905, 0.008491429629558585809, 0.01273714444433788305, 0.01698285925911717509, 0.02122857407389646886, 0.02547428888867576263, 0.02972000370345505293, 0.03396571851823434324 ),
 .UNSPECIFIED. ) ;
#10530 = CARTESIAN_POINT ( 'NONE',  ( -6.386751345947994984, 10.00000000000000355, -11.06217782649116366 ) ) ;
#10531 = DIRECTION ( 'NONE',  ( 0.000000000000000000, 1.000000000000000000, 0.000000000000000000 ) ) ;
#10532 = VERTEX_POINT ( 'NONE', #5842 ) ;
#10533 = EDGE_CURVE ( 'NONE', #4439, #9309, #9201, .T. ) ;
#10534 = EDGE_LOOP ( 'NONE', ( #1628, #1871, #10586, #676, #10374, #9242, #3672, #7171, #5425, #1393, #7169, #563, #6398, #5403 ) ) ;
#10535 =( GEOMETRIC_REPRESENTATION_CONTEXT ( 3 ) GLOBAL_UNCERTAINTY_ASSIGNED_CONTEXT ( ( #10683 ) ) GLOBAL_UNIT_ASSIGNED_CONTEXT ( ( #10605, #7185, #1280 ) ) REPRESENTATION_CONTEXT ( 'NONE', 'WORKASPACE' ) );
#10536 = FACE_OUTER_BOUND ( 'NONE', #5217, .T. ) ;
#10537 = DIRECTION ( 'NONE',  ( -0.9185586535436922606, 0.3535533905932755072, 0.1767766952966313421 ) ) ;
#10538 = DIRECTION ( 'NONE',  ( 0.000000000000000000, 0.000000000000000000, -1.000000000000000000 ) ) ;
#10539 = CARTESIAN_POINT ( 'NONE',  ( 6.386751345948060710, 10.00000000000000355, 11.06217782649112458 ) ) ;
#10540 = FACE_OUTER_BOUND ( 'NONE', #9978, .T. ) ;
#10541 = AXIS2_PLACEMENT_3D ( 'NONE', #8969, #7357, #7255 ) ;
#10542 = AXIS2_PLACEMENT_3D ( 'NONE', #2887, #308, #1302 ) ;
#10543 = VERTEX_POINT ( 'NONE', #542 ) ;
#10544 = VERTEX_POINT ( 'NONE', #7279 ) ;
#10545 = CARTESIAN_POINT ( 'NONE',  ( 0.000000000000000000, 88.00000000000001421, 6.000000000000000888 ) ) ;
#10546 = CARTESIAN_POINT ( 'NONE',  ( -9.875000000000143885, -0.001000000000001000089, -17.10400172474258085 ) ) ;
#10547 = CARTESIAN_POINT ( 'NONE',  ( -24.62111388750000174, 4.893749999044084475, -3.015216831376932151E-15 ) ) ;
#10548 = VERTEX_POINT ( 'NONE', #600 ) ;
#10549 = CARTESIAN_POINT ( 'NONE',  ( 24.81055694375000087, 0.1093749995220422710, 0.000000000000000000 ) ) ;
#10550 = FILL_AREA_STYLE_COLOUR ( '', #6308 ) ;
#10551 = CARTESIAN_POINT ( 'NONE',  ( 0.000000000000000000, -6.505213034913026604E-16, -1.154700538379252794 ) ) ;
#10552 = VECTOR ( 'NONE', #6825, 1000.000000000000000 ) ;
#10553 = CARTESIAN_POINT ( 'NONE',  ( -10.19839929293507375, 3.906249999044085097, 24.62111388749999108 ) ) ;
#10554 = CYLINDRICAL_SURFACE ( 'NONE', #331, 2.999999999999999112 ) ;
#10555 = ORIENTED_EDGE ( 'NONE', *, *, #1979, .T. ) ;
#10556 = ORIENTED_EDGE ( 'NONE', *, *, #130, .T. ) ;
#10557 = MANIFOLD_SOLID_BREP ( 'Cavity1', #9494 ) ;
#10558 = CIRCLE ( 'NONE', #1047, 4.999999999999987566 ) ;
#10559 = CYLINDRICAL_SURFACE ( 'NONE', #5318, 24.91176187412963117 ) ;
#10560 = CARTESIAN_POINT ( 'NONE',  ( 1.507608415688466075E-15, 3.468749999044085097, -24.62111388750000174 ) ) ;
#10561 = CARTESIAN_POINT ( 'NONE',  ( 24.62111388750000174, 4.393749999044085364, 0.000000000000000000 ) ) ;
#10562 = ADVANCED_FACE ( 'NONE', ( #6084 ), #1482, .F. ) ;
#10563 = CARTESIAN_POINT ( 'NONE',  ( 10.35533905932738286, 1.812500000000000222, 24.99999999999999645 ) ) ;
#10564 =( NAMED_UNIT ( * ) SI_UNIT ( $, .STERADIAN. ) SOLID_ANGLE_UNIT ( ) );
#10565 = DIRECTION ( 'NONE',  ( -0.8660254037844431485, 0.000000000000000000, -0.4999999999999922839 ) ) ;
#10566 = CARTESIAN_POINT ( 'NONE',  ( -11.42163336986836875, 7.781088913245557848, 7.171633369868196439 ) ) ;
#10567 = DIRECTION ( 'NONE',  ( 2.168404344971010594E-16, -0.000000000000000000, 1.000000000000000000 ) ) ;
#10568 = CARTESIAN_POINT ( 'NONE',  ( 24.99999999999999289, 0.9375000000000000000, 10.35533905932739529 ) ) ;
#10569 = CARTESIAN_POINT ( 'NONE',  ( 1.530808498934191521E-15, 2.250000000000000444, -25.00000000000000000 ) ) ;
#10570 = ADVANCED_FACE ( 'NONE', ( #10207 ), #2621, .F. ) ;
#10571 = ORIENTED_EDGE ( 'NONE', *, *, #8141, .T. ) ;
#10572 = EDGE_LOOP ( 'NONE', ( #4052, #2773, #3886, #5294, #2197, #4837 ) ) ;
#10573 = UNCERTAINTY_MEASURE_WITH_UNIT (LENGTH_MEASURE( 1.000000000000000082E-05 ), #4787, 'distance_accuracy_value', 'NONE');
#10574 = CARTESIAN_POINT ( 'NONE',  ( -10.35533905932737575, 0.3125000000000000000, -25.00000000000000000 ) ) ;
#10575 = EDGE_CURVE ( 'NONE', #9073, #9769, #1759, .T. ) ;
#10576 = DIRECTION ( 'NONE',  ( 0.000000000000000000, -2.775557561562888270E-17, -1.000000000000000000 ) ) ;
#10577 = EDGE_CURVE ( 'NONE', #7487, #3376, #3142, .T. ) ;
#10578 = CARTESIAN_POINT ( 'NONE',  ( 1.400000000000001910, 7.661233032048583711E-16, 5.100000000000006750 ) ) ;
#10579 = DIRECTION ( 'NONE',  ( -0.000000000000000000, -1.000000000000000000, -0.000000000000000000 ) ) ;
#10580 = DIRECTION ( 'NONE',  ( -0.8660254037844417052, 0.000000000000000000, -0.4999999999999947820 ) ) ;
#10581 = DIRECTION ( 'NONE',  ( 0.000000000000000000, -1.000000000000000000, 0.000000000000000000 ) ) ;
#10582 = DIRECTION ( 'NONE',  ( -0.000000000000000000, -1.000000000000000000, -0.000000000000000000 ) ) ;
#10583 = EDGE_CURVE ( 'NONE', #6763, #5070, #9377, .T. ) ;
#10584 = AXIS2_PLACEMENT_3D ( 'NONE', #1878, #8550, #998 ) ;
#10585 = VECTOR ( 'NONE', #3372, 999.9999999999998863 ) ;
#10586 = ORIENTED_EDGE ( 'NONE', *, *, #9276, .T. ) ;
#10587 = PRODUCT ( 'angular contact ball bearing_68_iso_ISO 15 ABB - 1710 - 20,SI,NC,20_68', 'angular contact ball bearing_68_iso_ISO 15 ABB - 1710 - 20,SI,NC,20_68', '', ( #707 ) ) ;
#10588 = CARTESIAN_POINT ( 'NONE',  ( 82.32050807568876394, 92.28203230275514102, 4.000000000000006217 ) ) ;
#10589 = LINE ( 'NONE', #8253, #761 ) ;
#10590 = DIRECTION ( 'NONE',  ( -1.000000000000000000, 8.326672684688672475E-15, 0.000000000000000000 ) ) ;
#10591 = AXIS2_PLACEMENT_3D ( 'NONE', #1101, #7717, #6902 ) ;
#10592 = EDGE_CURVE ( 'NONE', #10901, #6438, #938, .T. ) ;
#10593 = PLANE ( 'NONE',  #2157 ) ;
#10594 = CARTESIAN_POINT ( 'NONE',  ( 0.000000000000000000, 28.00000000000000000, 0.000000000000000000 ) ) ;
#10595 = EDGE_CURVE ( 'NONE', #10398, #3501, #5777, .T. ) ;
#10596 = VERTEX_POINT ( 'NONE', #2684 ) ;
#10597 = ORIENTED_EDGE ( 'NONE', *, *, #7355, .F. ) ;
#10598 = VECTOR ( 'NONE', #8856, 1000.000000000000000 ) ;
#10599 = AXIS2_PLACEMENT_3D ( 'NONE', #6793, #10149, #5841 ) ;
#10600 = PRESENTATION_STYLE_ASSIGNMENT (( #6619 ) ) ;
#10601 = CARTESIAN_POINT ( 'NONE',  ( 0.4330127018922225735, 0.000000000000000000, -0.2499999999999944766 ) ) ;
#10602 = CARTESIAN_POINT ( 'NONE',  ( 24.62111388749999108, 5.331249999044085364, 10.19839929293507730 ) ) ;
#10603 = ORIENTED_EDGE ( 'NONE', *, *, #8776, .F. ) ;
#10604 = DIRECTION ( 'NONE',  ( 0.4330127018922226290, 0.8660254037844380415, -0.2499999999999965028 ) ) ;
#10605 =( LENGTH_UNIT ( ) NAMED_UNIT ( * ) SI_UNIT ( .MILLI., .METRE. ) );
#10606 = DIRECTION ( 'NONE',  ( -1.000000000000000000, 0.000000000000000000, 0.000000000000000000 ) ) ;
#10607 = EDGE_CURVE ( 'NONE', #10522, #7535, #2769, .T. ) ;
#10608 = CARTESIAN_POINT ( 'NONE',  ( -10.19839929293505776, 2.531249999044085097, -24.62111388750000174 ) ) ;
#10609 = VERTEX_POINT ( 'NONE', #4186 ) ;
#10610 = CIRCLE ( 'NONE', #7253, 6.999999999999997335 ) ;
#10611 = EDGE_LOOP ( 'NONE', ( #4806, #1049, #18, #8468, #3483, #4459 ) ) ;
#10612 = CARTESIAN_POINT ( 'NONE',  ( -4.592425496802574367E-15, 3.362499998088169129, 25.00000000000000000 ) ) ;
#10613 = CARTESIAN_POINT ( 'NONE',  ( -10.19839929293507552, 4.906249999044083765, 24.62111388749999463 ) ) ;
#10614 = CARTESIAN_POINT ( 'NONE',  ( -24.62111388750000174, 1.831249999044084475, -10.19839929293506131 ) ) ;
#10615 = ORIENTED_EDGE ( 'NONE', *, *, #9343, .F. ) ;
#10616 = CARTESIAN_POINT ( 'NONE',  ( 10.35533905932737930, 4.187500000000000000, -25.00000000000000000 ) ) ;
#10617 =( NAMED_UNIT ( * ) PLANE_ANGLE_UNIT ( ) SI_UNIT ( $, .RADIAN. ) );
#10618 = CIRCLE ( 'NONE', #1616, 5.750000000000006217 ) ;
#10619 = DIRECTION ( 'NONE',  ( 0.000000000000000000, 0.000000000000000000, 1.000000000000000000 ) ) ;
#10620 = DIRECTION ( 'NONE',  ( 1.047444401652940007E-14, 0.000000000000000000, -1.000000000000000000 ) ) ;
#10621 = LINE ( 'NONE', #10678, #9561 ) ;
#10622 = LINE ( 'NONE', #5869, #10228 ) ;
#10623 = VECTOR ( 'NONE', #2897, 1000.000000000000114 ) ;
#10624 = ORIENTED_EDGE ( 'NONE', *, *, #3463, .T. ) ;
#10625 = ORIENTED_EDGE ( 'NONE', *, *, #7281, .T. ) ;
#10626 = CIRCLE ( 'NONE', #2331, 2.999999999999997335 ) ;
#10627 = CARTESIAN_POINT ( 'NONE',  ( -25.00000000000000000, 0.4374999999999999445, -10.35533905932738108 ) ) ;
#10628 = AXIS2_PLACEMENT_3D ( 'NONE', #3443, #3564, #10419 ) ;
#10629 = DIRECTION ( 'NONE',  ( 0.000000000000000000, 1.000000000000000000, 0.000000000000000000 ) ) ;
#10630 = CARTESIAN_POINT ( 'NONE',  ( 1.530808498934191521E-15, 1.862499998088169129, -25.00000000000000000 ) ) ;
#10631 = AXIS2_PLACEMENT_3D ( 'NONE', #5721, #4889, #6603 ) ;
#10632 = CARTESIAN_POINT ( 'NONE',  ( -4.592425496802574367E-15, 4.362499998088169129, 25.00000000000000000 ) ) ;
#10633 = ORIENTED_EDGE ( 'NONE', *, *, #7656, .T. ) ;
#10634 = DIRECTION ( 'NONE',  ( -0.000000000000000000, -1.000000000000000000, -0.000000000000000000 ) ) ;
#10635 = CARTESIAN_POINT ( 'NONE',  ( -1.500000000000000444, 83.00000000000000000, -1.500000000000000222 ) ) ;
#10636 = AXIS2_PLACEMENT_3D ( 'NONE', #5998, #5112, #5066 ) ;
#10637 = DIRECTION ( 'NONE',  ( 1.000000000000000000, 0.000000000000000000, -0.000000000000000000 ) ) ;
#10638 = CARTESIAN_POINT ( 'NONE',  ( -10.35533905932739174, 3.687500000000000444, 24.99999999999999289 ) ) ;
#10639 = EDGE_CURVE ( 'NONE', #10668, #3974, #8950, .T. ) ;
#10640 = EDGE_CURVE ( 'NONE', #8568, #9592, #8042, .T. ) ;
#10641 = AXIS2_PLACEMENT_3D ( 'NONE', #9672, #5270, #2097 ) ;
#10642 = VERTEX_POINT ( 'NONE', #10327 ) ;
#10643 = VECTOR ( 'NONE', #5513, 1000.000000000000000 ) ;
#10644 = EDGE_LOOP ( 'NONE', ( #7740, #9036, #1686, #8913, #793, #7324 ) ) ;
#10645 = VECTOR ( 'NONE', #3073, 999.9999999999998863 ) ;
#10646 = ADVANCED_FACE ( 'NONE', ( #2739 ), #822, .F. ) ;
#10647 = DIRECTION ( 'NONE',  ( -0.8660254037844415942, 0.000000000000000000, 0.4999999999999949485 ) ) ;
#10648 = AXIS2_PLACEMENT_3D ( 'NONE', #8879, #3853, #1314 ) ;
#10649 = CARTESIAN_POINT ( 'NONE',  ( 67.97877056362573001, 94.28203230275514102, 5.000000000000000000 ) ) ;
#10650 = CARTESIAN_POINT ( 'NONE',  ( 24.99999999999999289, 4.549999998088169129, 10.35533905932739529 ) ) ;
#10651 = CARTESIAN_POINT ( 'NONE',  ( 17.67766952966369232, 1.125000000000000222, -17.67766952966369232 ) ) ;
#10652 = LINE ( 'NONE', #5572, #1283 ) ;
#10653 = AXIS2_PLACEMENT_3D ( 'NONE', #3217, #9973, #9141 ) ;
#10654 = ADVANCED_FACE ( 'NONE', ( #7604 ), #37, .F. ) ;
#10655 = ORIENTED_EDGE ( 'NONE', *, *, #10592, .F. ) ;
#10656 = ORIENTED_EDGE ( 'NONE', *, *, #3909, .F. ) ;
#10657 = EDGE_CURVE ( 'NONE', #4468, #8291, #10375, .T. ) ;
#10658 = CARTESIAN_POINT ( 'NONE',  ( -12.13990010960501031, 28.00000000000000000, -10.47307621135320410 ) ) ;
#10659 = CARTESIAN_POINT ( 'NONE',  ( 0.000000000000000000, 5.000000000000000000, -22.00000000000000355 ) ) ;
#10660 = CARTESIAN_POINT ( 'NONE',  ( -17.40975659021753330, 2.018749999044084475, 17.40975659021752975 ) ) ;
#10661 = EDGE_LOOP ( 'NONE', ( #7930, #2312, #84, #3409 ) ) ;
#10662 = DIRECTION ( 'NONE',  ( -0.8660254037844432595, 0.000000000000000000, 0.4999999999999919509 ) ) ;
#10663 = DIRECTION ( 'NONE',  ( 0.000000000000000000, 0.000000000000000000, 1.000000000000000000 ) ) ;
#10664 = CARTESIAN_POINT ( 'NONE',  ( 7.347880794884118750E-16, 28.00000000000000000, 5.999999999999999112 ) ) ;
#10665 = ORIENTED_EDGE ( 'NONE', *, *, #6940, .T. ) ;
#10666 = DIRECTION ( 'NONE',  ( 0.000000000000000000, -0.000000000000000000, 1.000000000000000000 ) ) ;
#10667 = CARTESIAN_POINT ( 'NONE',  ( -10.19839929293507375, 0.9062499990440844311, 24.62111388749999108 ) ) ;
#10668 = VERTEX_POINT ( 'NONE', #10379 ) ;
#10669 = EDGE_LOOP ( 'NONE', ( #1484, #2006, #8770, #2131 ) ) ;
#10670 = CARTESIAN_POINT ( 'NONE',  ( 10.35533905932737930, 4.799999998088169129, -25.00000000000000000 ) ) ;
#10671 = CYLINDRICAL_SURFACE ( 'NONE', #4957, 7.500000000000007994 ) ;
#10672 = CARTESIAN_POINT ( 'NONE',  ( -24.62111388750000174, 2.893749999044084475, -3.015216831376932151E-15 ) ) ;
#10673 = VERTEX_POINT ( 'NONE', #7072 ) ;
#10674 = FACE_OUTER_BOUND ( 'NONE', #9190, .T. ) ;
#10675 = SURFACE_SIDE_STYLE ('',( #2108 ) ) ;
#10676 = CARTESIAN_POINT ( 'NONE',  ( -7.276923788646840308, 28.00000000000000000, -18.60400172474260216 ) ) ;
#10677 = CARTESIAN_POINT ( 'NONE',  ( 0.4330127018922172999, 0.000000000000000000, 0.2500000000000036082 ) ) ;
#10678 = CARTESIAN_POINT ( 'NONE',  ( 1.499999999999999556, 88.00000000000001421, -1.500000000000000222 ) ) ;
#10679 = DIRECTION ( 'NONE',  ( -0.5000000000000039968, 0.000000000000000000, 0.8660254037844363761 ) ) ;
#10680 = ORIENTED_EDGE ( 'NONE', *, *, #50, .F. ) ;
#10681 = ORIENTED_EDGE ( 'NONE', *, *, #6350, .F. ) ;
#10682 = ORIENTED_EDGE ( 'NONE', *, *, #2321, .F. ) ;
#10683 = UNCERTAINTY_MEASURE_WITH_UNIT (LENGTH_MEASURE( 1.000000000000000082E-05 ), #10605, 'distance_accuracy_value', 'NONE');
#10684 = CARTESIAN_POINT ( 'NONE',  ( 10.35533905932738286, 3.812500000000000000, 24.99999999999999645 ) ) ;
#10685 = CARTESIAN_POINT ( 'NONE',  ( -17.67766952966368876, 4.375000000000000000, -17.67766952966369232 ) ) ;
#10686 = DIRECTION ( 'NONE',  ( -0.000000000000000000, -0.000000000000000000, 1.000000000000000000 ) ) ;
#10687 = ORIENTED_EDGE ( 'NONE', *, *, #10774, .F. ) ;
#10688 = DIRECTION ( 'NONE',  ( 0.000000000000000000, -1.000000000000000000, 0.000000000000000000 ) ) ;
#10689 = CARTESIAN_POINT ( 'NONE',  ( -7.276923788646448621, 28.00000000000000000, 18.60400172474275848 ) ) ;
#10690 = CARTESIAN_POINT ( 'NONE',  ( -4.522825247065398226E-15, 0.9687499990440845421, 24.62111388750000174 ) ) ;
#10691 = LINE ( 'NONE', #523, #3938 ) ;
#10692 = ORIENTED_EDGE ( 'NONE', *, *, #5831, .T. ) ;
#10693 = ORIENTED_EDGE ( 'NONE', *, *, #1928, .T. ) ;
#10694 = ORIENTED_EDGE ( 'NONE', *, *, #2451, .T. ) ;
#10695 = CARTESIAN_POINT ( 'NONE',  ( -18.60400172474257730, 28.00000000000000000, 7.276923788646904256 ) ) ;
#10696 = EDGE_CURVE ( 'NONE', #9174, #10609, #1614, .T. ) ;
#10697 = CARTESIAN_POINT ( 'NONE',  ( 6.386751345948143310, 10.00000000000000355, -11.06217782649107839 ) ) ;
#10698 = DIRECTION ( 'NONE',  ( 0.000000000000000000, 1.000000000000000000, 0.000000000000000000 ) ) ;
#10699 = CARTESIAN_POINT ( 'NONE',  ( 4.336808689942017736E-16, 20.00000000000000355, -6.999999999999997335 ) ) ;
#10700 = EDGE_CURVE ( 'NONE', #2786, #634, #7850, .T. ) ;
#10701 = ORIENTED_EDGE ( 'NONE', *, *, #3989, .T. ) ;
#10702 = CARTESIAN_POINT ( 'NONE',  ( -10.00000000000000000, 90.00000000000001421, 5.000000000000000000 ) ) ;
#10703 = DIRECTION ( 'NONE',  ( 0.8660254037844361541, 0.000000000000000000, -0.5000000000000042188 ) ) ;
#10704 =( LENGTH_UNIT ( ) NAMED_UNIT ( * ) SI_UNIT ( .MILLI., .METRE. ) );
#10705 = CARTESIAN_POINT ( 'NONE',  ( 10.19839929293506486, 2.206249999044084920, 24.62111388749999819 ) ) ;
#10706 = ORIENTED_EDGE ( 'NONE', *, *, #5259, .T. ) ;
#10707 = EDGE_CURVE ( 'NONE', #6463, #5838, #5839, .T. ) ;
#10708 = CARTESIAN_POINT ( 'NONE',  ( 0.000000000000000000, 10.10000000000000497, 0.000000000000000000 ) ) ;
#10709 = DIRECTION ( 'NONE',  ( 0.000000000000000000, 1.000000000000000000, 0.000000000000000000 ) ) ;
#10710 = DIRECTION ( 'NONE',  ( 0.000000000000000000, 1.000000000000000000, 0.000000000000000000 ) ) ;
#10711 = CARTESIAN_POINT ( 'NONE',  ( 16.00000000000000000, 0.000000000000000000, 0.000000000000000000 ) ) ;
#10712 = CARTESIAN_POINT ( 'NONE',  ( 17.40975659021752975, 1.343749999044084653, -17.40975659021752975 ) ) ;
#10713 = EDGE_CURVE ( 'NONE', #1976, #564, #5773, .T. ) ;
#10714 = ORIENTED_EDGE ( 'NONE', *, *, #3323, .T. ) ;
#10715 = COLOUR_RGB ( '', 0.72549020, 0.75294118, 0.79215686) ;
#10716 = CARTESIAN_POINT ( 'NONE',  ( -17.67766952966369232, 5.237499998088169129, 17.67766952966368876 ) ) ;
#10717 = CYLINDRICAL_SURFACE ( 'NONE', #8461, 5.525000000000006573 ) ;
#10718 = AXIS2_PLACEMENT_3D ( 'NONE', #6531, #10840, #3239 ) ;
#10719 = CARTESIAN_POINT ( 'NONE',  ( -17.40975659021752975, 3.593749999044084653, -17.40975659021752975 ) ) ;
#10720 = ORIENTED_EDGE ( 'NONE', *, *, #1610, .T. ) ;
#10721 = CARTESIAN_POINT ( 'NONE',  ( 1.530808498934191521E-15, 3.250000000000000444, -25.00000000000000000 ) ) ;
#10722 = SHAPE_REPRESENTATION_RELATIONSHIP ( 'NONE' , 'NONE' ,  #6555, #10206 ) ;
#10723 = DIRECTION ( 'NONE',  ( 0.000000000000000000, 0.000000000000000000, 1.000000000000000000 ) ) ;
#10724 = CARTESIAN_POINT ( 'NONE',  ( -17.67766952966368876, 1.987499998088169129, -17.67766952966369232 ) ) ;
#10725 = CYLINDRICAL_SURFACE ( 'NONE', #5347, 4.999999999999987566 ) ;
#10726 = DIRECTION ( 'NONE',  ( -0.000000000000000000, -0.000000000000000000, 1.000000000000000000 ) ) ;
#10727 = VECTOR ( 'NONE', #8405, 1000.000000000000000 ) ;
#10728 = EDGE_CURVE ( 'NONE', #10381, #9593, #1456, .T. ) ;
#10729 = CIRCLE ( 'NONE', #6859, 2.999999999999996891 ) ;
#10730 = ORIENTED_EDGE ( 'NONE', *, *, #4118, .T. ) ;
#10731 = ORIENTED_EDGE ( 'NONE', *, *, #7663, .F. ) ;
#10732 = ORIENTED_EDGE ( 'NONE', *, *, #9019, .T. ) ;
#10733 = MANIFOLD_SOLID_BREP ( 'Revolve1', #138 ) ;
#10734 = CARTESIAN_POINT ( 'NONE',  ( 10.35533905932737930, 3.187500000000000444, -25.00000000000000000 ) ) ;
#10735 = CARTESIAN_POINT ( 'NONE',  ( 10.35533905932738641, 1.799999998088168685, -24.99999999999999289 ) ) ;
#10736 = ORIENTED_EDGE ( 'NONE', *, *, #2398, .F. ) ;
#10737 = FACE_OUTER_BOUND ( 'NONE', #5567, .T. ) ;
#10738 = LINE ( 'NONE', #2229, #6735 ) ;
#10739 = CARTESIAN_POINT ( 'NONE',  ( 24.62111388750000174, 1.281249999044084653, -10.19839929293505776 ) ) ;
#10740 = DIRECTION ( 'NONE',  ( 0.000000000000000000, 0.000000000000000000, -1.000000000000000000 ) ) ;
#10741 = VERTEX_POINT ( 'NONE', #5665 ) ;
#10742 = ORIENTED_EDGE ( 'NONE', *, *, #8543, .F. ) ;
#10743 = VERTEX_POINT ( 'NONE', #9023 ) ;
#10744 = CARTESIAN_POINT ( 'NONE',  ( -18.60400172474273361, 28.00000000000000000, -7.276923788646511682 ) ) ;
#10745 = LINE ( 'NONE', #2352, #7290 ) ;
#10746 = DIRECTION ( 'NONE',  ( 0.000000000000000000, 0.000000000000000000, 1.000000000000000000 ) ) ;
#10747 = DIRECTION ( 'NONE',  ( 0.000000000000000000, 0.000000000000000000, 1.000000000000000000 ) ) ;
#10748 = CARTESIAN_POINT ( 'NONE',  ( 3.500000000000004885, 20.00000000000000355, -6.062177826491062405 ) ) ;
#10749 = AXIS2_PLACEMENT_3D ( 'NONE', #1107, #570, #6971 ) ;
#10750 = CIRCLE ( 'NONE', #6004, 2.999999999999999112 ) ;
#10751 = ORIENTED_EDGE ( 'NONE', *, *, #9260, .T. ) ;
#10752 = ADVANCED_FACE ( 'NONE', ( #8192 ), #9496, .T. ) ;
#10753 = EDGE_CURVE ( 'NONE', #9293, #7845, #9608, .T. ) ;
#10754 = ORIENTED_EDGE ( 'NONE', *, *, #8538, .T. ) ;
#10755 = AXIS2_PLACEMENT_3D ( 'NONE', #3650, #7034, #10662 ) ;
#10756 = PLANE ( 'NONE',  #8250 ) ;
#10757 = CARTESIAN_POINT ( 'NONE',  ( 7.856406460551036197, 93.00000000000001421, -5.000000000000000000 ) ) ;
#10758 =( NAMED_UNIT ( * ) PLANE_ANGLE_UNIT ( ) SI_UNIT ( $, .RADIAN. ) );
#10759 = VECTOR ( 'NONE', #4257, 1000.000000000000000 ) ;
#10760 = CARTESIAN_POINT ( 'NONE',  ( 24.62111388750000174, 4.393749999044084475, 0.000000000000000000 ) ) ;
#10761 = ORIENTED_EDGE ( 'NONE', *, *, #10242, .F. ) ;
#10762 = DIRECTION ( 'NONE',  ( -0.6123724356957948034, -0.3535533905932734533, 0.7071067811865474617 ) ) ;
#10763 = DIRECTION ( 'NONE',  ( 1.000000000000000000, 0.000000000000000000, 0.000000000000000000 ) ) ;
#10764 = CARTESIAN_POINT ( 'NONE',  ( -1.135781565508698732E-14, 10.00000000000000355, -12.77350269189627241 ) ) ;
#10765 = EDGE_LOOP ( 'NONE', ( #1164, #3438, #9017, #7662 ) ) ;
#10766 = CARTESIAN_POINT ( 'NONE',  ( -4.592425496802574367E-15, 1.750000000000000000, 25.00000000000000000 ) ) ;
#10767 = CARTESIAN_POINT ( 'NONE',  ( -10.19839929293505776, 1.531249999044084653, -24.62111388750000174 ) ) ;
#10768 = VECTOR ( 'NONE', #4587, 1000.000000000000000 ) ;
#10769 = ORIENTED_EDGE ( 'NONE', *, *, #10789, .T. ) ;
#10770 = EDGE_CURVE ( 'NONE', #5226, #8103, #672, .T. ) ;
#10771 = EDGE_CURVE ( 'NONE', #2468, #7097, #518, .T. ) ;
#10772 = MANIFOLD_SOLID_BREP ( 'Hex', #3286 ) ;
#10773 = EDGE_LOOP ( 'NONE', ( #1293, #6908, #8369, #5421 ) ) ;
#10774 = EDGE_CURVE ( 'NONE', #915, #10157, #7415, .T. ) ;
#10775 = CARTESIAN_POINT ( 'NONE',  ( 17.67766952966368521, 4.487499998088169129, 17.67766952966369232 ) ) ;
#10776 = CYLINDRICAL_SURFACE ( 'NONE', #9539, 2.999999999999997335 ) ;
#10777 = CARTESIAN_POINT ( 'NONE',  ( 17.40975659021752620, 1.093749999044084653, 17.40975659021753330 ) ) ;
#10778 = ORIENTED_EDGE ( 'NONE', *, *, #4227, .T. ) ;
#10779 = DIRECTION ( 'NONE',  ( 0.000000000000000000, 1.000000000000000000, 0.000000000000000000 ) ) ;
#10780 = EDGE_CURVE ( 'NONE', #1987, #7845, #6770, .T. ) ;
#10781 = VECTOR ( 'NONE', #10010, 1000.000000000000114 ) ;
#10782 =( BOUNDED_CURVE ( )  B_SPLINE_CURVE ( 3, ( #7819, #1145, #6165, #3666 ),
 .UNSPECIFIED., .F., .F. ) 
 B_SPLINE_CURVE_WITH_KNOTS ( ( 4, 4 ),
 ( 2.284520705739657931, 2.356010155625176683 ),
 .UNSPECIFIED. ) 
 CURVE ( )  GEOMETRIC_REPRESENTATION_ITEM ( )  RATIONAL_B_SPLINE_CURVE ( ( 1.000000000000000000, 0.9995741502243209453, 0.9995741502243209453, 1.000000000000000000 ) ) 
 REPRESENTATION_ITEM ( '' )  );
#10783 = FACE_OUTER_BOUND ( 'NONE', #10064, .T. ) ;
#10784 = DIRECTION ( 'NONE',  ( 0.000000000000000000, 0.000000000000000000, -1.000000000000000000 ) ) ;
#10785 = CARTESIAN_POINT ( 'NONE',  ( 67.32050807568876394, 92.28203230275514102, -5.000000000000000000 ) ) ;
#10786 = DIRECTION ( 'NONE',  ( 0.000000000000000000, 0.8660254037844391517, 0.4999999999999992228 ) ) ;
#10787 = AXIS2_PLACEMENT_3D ( 'NONE', #9687, #10468, #1388 ) ;
#10788 = EDGE_LOOP ( 'NONE', ( #9072, #5346, #2961, #7943 ) ) ;
#10789 = EDGE_CURVE ( 'NONE', #6450, #4041, #6855, .T. ) ;
#10790 = ORIENTED_EDGE ( 'NONE', *, *, #1464, .T. ) ;
#10791 = ORIENTED_EDGE ( 'NONE', *, *, #3632, .T. ) ;
#10792 = ORIENTED_EDGE ( 'NONE', *, *, #994, .F. ) ;
#10793 = PRODUCT_DEFINITION_CONTEXT ( 'detailed design', #7440, 'design' ) ;
#10794 = AXIS2_PLACEMENT_3D ( 'NONE', #3189, #3997, #2478 ) ;
#10795 = CARTESIAN_POINT ( 'NONE',  ( 0.000000000000000000, 88.00000000000001421, 0.000000000000000000 ) ) ;
#10796 = DIRECTION ( 'NONE',  ( 0.000000000000000000, -0.000000000000000000, -1.000000000000000000 ) ) ;
#10797 = EDGE_CURVE ( 'NONE', #1630, #689, #737, .T. ) ;
#10798 = ORIENTED_EDGE ( 'NONE', *, *, #10583, .T. ) ;
#10799 = VECTOR ( 'NONE', #3001, 1000.000000000000000 ) ;
#10800 = CARTESIAN_POINT ( 'NONE',  ( 0.000000000000000000, 25.00000000000000355, 0.000000000000000000 ) ) ;
#10801 = DIRECTION ( 'NONE',  ( 0.000000000000000000, 1.000000000000000000, 0.000000000000000000 ) ) ;
#10802 = CARTESIAN_POINT ( 'NONE',  ( 24.62111388750000174, 4.218749999044084653, 0.000000000000000000 ) ) ;
#10803 = DIRECTION ( 'NONE',  ( 0.000000000000000000, 0.000000000000000000, 1.000000000000000000 ) ) ;
#10804 = CIRCLE ( 'NONE', #8692, 2.999999999999997780 ) ;
#10805 = ORIENTED_EDGE ( 'NONE', *, *, #8713, .F. ) ;
#10806 = VERTEX_POINT ( 'NONE', #11 ) ;
#10807 = AXIS2_PLACEMENT_3D ( 'NONE', #2499, #8476, #8371 ) ;
#10808 = ORIENTED_EDGE ( 'NONE', *, *, #3331, .T. ) ;
#10809 = ADVANCED_FACE ( 'NONE', ( #3252, #8238 ), #6650, .F. ) ;
#10810 = VECTOR ( 'NONE', #10860, 1000.000000000000000 ) ;
#10811 = DIRECTION ( 'NONE',  ( -0.4330127018922172999, -0.8660254037844380415, -0.2500000000000055511 ) ) ;
#10812 = CARTESIAN_POINT ( 'NONE',  ( 0.000000000000000000, -0.5289809421253948152, 0.000000000000000000 ) ) ;
#10813 = CARTESIAN_POINT ( 'NONE',  ( -4.592425496802574367E-15, 4.750000000000000000, 25.00000000000000000 ) ) ;
#10814 = CARTESIAN_POINT ( 'NONE',  ( 17.67766952966369232, 4.125000000000000000, -17.67766952966369232 ) ) ;
#10815 = DIRECTION ( 'NONE',  ( -1.000000000000000000, 0.000000000000000000, 0.000000000000000000 ) ) ;
#10816 = AXIS2_PLACEMENT_3D ( 'NONE', #7864, #4510, #7802 ) ;
#10817 = AXIS2_PLACEMENT_3D ( 'NONE', #115, #7686, #1068 ) ;
#10818 = CIRCLE ( 'NONE', #4488, 5.100000000000006750 ) ;
#10819 = ORIENTED_EDGE ( 'NONE', *, *, #792, .T. ) ;
#10820 = AXIS2_PLACEMENT_3D ( 'NONE', #5778, #754, #7542 ) ;
#10821 = AXIS2_PLACEMENT_3D ( 'NONE', #3569, #9194, #10368 ) ;
#10822 = SURFACE_STYLE_FILL_AREA ( #8167 ) ;
#10823 = DIRECTION ( 'NONE',  ( -0.000000000000000000, 1.000000000000000000, -0.000000000000000000 ) ) ;
#10824 = CARTESIAN_POINT ( 'NONE',  ( -24.62111388750000174, 0.8937499990440845865, -3.015216831376932151E-15 ) ) ;
#10825 = DIRECTION ( 'NONE',  ( -0.000000000000000000, -1.000000000000000000, -0.000000000000000000 ) ) ;
#10826 = DIRECTION ( 'NONE',  ( 1.000000000000000000, 0.000000000000000000, 0.000000000000000000 ) ) ;
#10827 = CARTESIAN_POINT ( 'NONE',  ( 0.000000000000000000, 31.00000000000000000, 0.000000000000000000 ) ) ;
#10828 = AXIS2_PLACEMENT_3D ( 'NONE', #4033, #8173, #2204 ) ;
#10829 = CARTESIAN_POINT ( 'NONE',  ( 0.5000000000000000000, 10.00000000000000355, -6.982120021884467675 ) ) ;
#10830 = ORIENTED_EDGE ( 'NONE', *, *, #7732, .T. ) ;
#10831 = CIRCLE ( 'NONE', #4131, 25.00000000000000000 ) ;
#10832 = ORIENTED_EDGE ( 'NONE', *, *, #10030, .F. ) ;
#10833 = CARTESIAN_POINT ( 'NONE',  ( 25.00000000000000000, 3.674999998088170017, -10.35533905932737753 ) ) ;
#10834 = CARTESIAN_POINT ( 'NONE',  ( 1.507608415688466075E-15, 1.468749999044084431, -24.62111388750000174 ) ) ;
#10835 = DIRECTION ( 'NONE',  ( -0.8660254037844399289, 0.000000000000000000, -0.4999999999999977796 ) ) ;
#10836 = EDGE_LOOP ( 'NONE', ( #5703, #1913, #4128, #3980 ) ) ;
#10837 = DIRECTION ( 'NONE',  ( -0.8660254037844328234, 0.000000000000000000, -0.5000000000000101030 ) ) ;
#10838 = DIRECTION ( 'NONE',  ( -1.000000000000000000, 0.000000000000000000, 1.445602896647339163E-16 ) ) ;
#10839 = ADVANCED_FACE ( 'NONE', ( #4057 ), #4216, .T. ) ;
#10840 = DIRECTION ( 'NONE',  ( -0.9185586535436915945, -0.3535533905932732868, -0.1767766952966388083 ) ) ;
#10841 = CARTESIAN_POINT ( 'NONE',  ( 0.000000000000000000, 20.00000000000000355, 0.000000000000000000 ) ) ;
#10842 = CARTESIAN_POINT ( 'NONE',  ( -9.875000000000143885, 28.00000000000000000, -17.10400172474258085 ) ) ;
#10843 = LINE ( 'NONE', #1780, #1575 ) ;
#10844 = EDGE_CURVE ( 'NONE', #7005, #10105, #4276, .T. ) ;
#10845 =( REPRESENTATION_RELATIONSHIP ('NONE','NONE', #1269, #4232 ) REPRESENTATION_RELATIONSHIP_WITH_TRANSFORMATION ( #877 )SHAPE_REPRESENTATION_RELATIONSHIP( ) );
#10846 = VERTEX_POINT ( 'NONE', #1559 ) ;
#10847 = ORIENTED_EDGE ( 'NONE', *, *, #1066, .F. ) ;
#10848 = EDGE_CURVE ( 'NONE', #8291, #8513, #2542, .T. ) ;
#10849 = ORIENTED_EDGE ( 'NONE', *, *, #66, .F. ) ;
#10850 =( BOUNDED_CURVE ( )  B_SPLINE_CURVE ( 2, ( #10909, #9182, #4280, #1620, #5008, #2544, #5109, #3433, #4217 ),
 .UNSPECIFIED., .F., .F. ) 
 B_SPLINE_CURVE_WITH_KNOTS ( ( 3, 2, 2, 2, 3 ),
 ( 0.2499999999999999722, 0.2750000000000000222, 0.2999999999999999889, 0.3250000000000000111, 0.3499999999999999778 ),
 .UNSPECIFIED. ) 
 CURVE ( )  GEOMETRIC_REPRESENTATION_ITEM ( )  RATIONAL_B_SPLINE_CURVE ( ( 1.000000000000000000, 0.9238795325112866275, 1.000000000000000000, 0.9238795325112867385, 1.000000000000000000, 0.9238795325112867385, 1.000000000000000000, 0.9238795325112867385, 1.000000000000000000 ) ) 
 REPRESENTATION_ITEM ( '' )  );
#10851 = CARTESIAN_POINT ( 'NONE',  ( -17.40975659021752975, 0.7687499990440845865, -17.40975659021752975 ) ) ;
#10852 = CARTESIAN_POINT ( 'NONE',  ( -10.19839929293505776, 1.531249999044084653, -24.62111388750000174 ) ) ;
#10853 = DIRECTION ( 'NONE',  ( 0.000000000000000000, -1.000000000000000000, 2.775557561562888270E-17 ) ) ;
#10854 = ORIENTED_EDGE ( 'NONE', *, *, #1696, .F. ) ;
#10855 = EDGE_CURVE ( 'NONE', #1858, #500, #5617, .T. ) ;
#10856 = CARTESIAN_POINT ( 'NONE',  ( 0.2500000000000050515, 0.000000000000000000, -0.4330127018922164117 ) ) ;
#10857 = DIRECTION ( 'NONE',  ( 0.000000000000000000, 1.000000000000000000, 0.000000000000000000 ) ) ;
#10858 = FACE_OUTER_BOUND ( 'NONE', #5554, .T. ) ;
#10859 = CARTESIAN_POINT ( 'NONE',  ( -4.522825247065398226E-15, 1.968749999044084653, 24.62111388750000174 ) ) ;
#10860 = DIRECTION ( 'NONE',  ( -1.000000000000000000, 0.000000000000000000, 1.069128445102650095E-14 ) ) ;
#10861 = VERTEX_POINT ( 'NONE', #4945 ) ;
#10862 = ORIENTED_EDGE ( 'NONE', *, *, #436, .T. ) ;
#10863 = ORIENTED_EDGE ( 'NONE', *, *, #4969, .F. ) ;
#10864 = VERTEX_POINT ( 'NONE', #3307 ) ;
#10865 = EDGE_CURVE ( 'NONE', #7330, #6845, #10384, .T. ) ;
#10866 = ORIENTED_EDGE ( 'NONE', *, *, #2267, .T. ) ;
#10867 = ORIENTED_EDGE ( 'NONE', *, *, #7953, .T. ) ;
#10868 = CARTESIAN_POINT ( 'NONE',  ( 10.19839929293506486, 2.206249999044084920, 24.62111388749999819 ) ) ;
#10869 = DIRECTION ( 'NONE',  ( 1.000000000000000000, 0.000000000000000000, 0.000000000000000000 ) ) ;
#10870 = PLANE ( 'NONE',  #3395 ) ;
#10871 = DIRECTION ( 'NONE',  ( -0.000000000000000000, 1.000000000000000000, -0.000000000000000000 ) ) ;
#10872 = CARTESIAN_POINT ( 'NONE',  ( 25.00000000000000000, 0.06249999999999997224, -10.35533905932737753 ) ) ;
#10873 = CARTESIAN_POINT ( 'NONE',  ( 22.03074295656257320, 5.000000000000000000, 11.55328354274170444 ) ) ;
#10874 = EDGE_CURVE ( 'NONE', #5240, #1695, #6710, .T. ) ;
#10875 = ORIENTED_EDGE ( 'NONE', *, *, #3248, .T. ) ;
#10876 = DIRECTION ( 'NONE',  ( -0.000000000000000000, 1.000000000000000000, 0.000000000000000000 ) ) ;
#10877 = DIRECTION ( 'NONE',  ( 0.000000000000000000, 1.000000000000000000, 0.000000000000000000 ) ) ;
#10878 = DIRECTION ( 'NONE',  ( -0.000000000000000000, 1.000000000000000000, -0.000000000000000000 ) ) ;
#10879 = ORIENTED_EDGE ( 'NONE', *, *, #377, .F. ) ;
#10880 = DIRECTION ( 'NONE',  ( -1.000000000000000000, 0.000000000000000000, 0.000000000000000000 ) ) ;
#10881 = DIRECTION ( 'NONE',  ( 0.000000000000000000, 0.000000000000000000, 1.000000000000000000 ) ) ;
#10882 = LINE ( 'NONE', #5084, #7456 ) ;
#10883 = CARTESIAN_POINT ( 'NONE',  ( 0.000000000000000000, 10.00000000000000355, 0.000000000000000000 ) ) ;
#10884 = CARTESIAN_POINT ( 'NONE',  ( 10.19839929293505953, 2.406249999044085541, -24.62111388750000174 ) ) ;
#10885 = ORIENTED_EDGE ( 'NONE', *, *, #7900, .T. ) ;
#10886 = ORIENTED_EDGE ( 'NONE', *, *, #997, .T. ) ;
#10887 = CARTESIAN_POINT ( 'NONE',  ( 24.62111388749999463, 4.331249999044084475, 10.19839929293507730 ) ) ;
#10888 = CARTESIAN_POINT ( 'NONE',  ( -13.63990010960498367, -0.001000000000001000089, -7.874999999999870326 ) ) ;
#10889 = STYLED_ITEM ( 'NONE', ( #4662 ), #9142 ) ;
#10890 = CARTESIAN_POINT ( 'NONE',  ( -17.40975659021753330, 2.843749999044085097, 17.40975659021752975 ) ) ;
#10891 = CARTESIAN_POINT ( 'NONE',  ( 7.856406460551036197, 98.00000000000001421, 5.000000000000000000 ) ) ;
#10892 = VERTEX_POINT ( 'NONE', #800 ) ;
#10893 = DIRECTION ( 'NONE',  ( 0.000000000000000000, 0.000000000000000000, 1.000000000000000000 ) ) ;
#10894 = FILL_AREA_STYLE_COLOUR ( '', #8231 ) ;
#10895 = CARTESIAN_POINT ( 'NONE',  ( 0.000000000000000000, -1.000000000000003109, -0.5773502691896260641 ) ) ;
#10896 = LINE ( 'NONE', #9011, #1743 ) ;
#10897 = DIRECTION ( 'NONE',  ( -0.000000000000000000, -1.000000000000000000, -0.000000000000000000 ) ) ;
#10898 = CARTESIAN_POINT ( 'NONE',  ( 7.276923788646575630, 25.00000000000000000, -18.60400172474270519 ) ) ;
#10899 = ORIENTED_EDGE ( 'NONE', *, *, #3962, .F. ) ;
#10900 = STYLED_ITEM ( 'NONE', ( #8989 ), #10557 ) ;
#10901 = VERTEX_POINT ( 'NONE', #4166 ) ;
#10902 = ORIENTED_EDGE ( 'NONE', *, *, #2932, .F. ) ;
#10903 = ORIENTED_EDGE ( 'NONE', *, *, #10471, .T. ) ;
#10904 = EDGE_CURVE ( 'NONE', #7447, #8872, #8633, .T. ) ;
#10905 = CARTESIAN_POINT ( 'NONE',  ( -24.62111388750000174, 0.8312499990440843645, -10.19839929293506131 ) ) ;
#10906 = CARTESIAN_POINT ( 'NONE',  ( -17.40975659021752975, 1.593749999044084431, -17.40975659021752975 ) ) ;
#10907 =( NAMED_UNIT ( * ) SI_UNIT ( $, .STERADIAN. ) SOLID_ANGLE_UNIT ( ) );
#10908 = EDGE_LOOP ( 'NONE', ( #1503, #9086, #8249, #3820 ) ) ;
#10909 = CARTESIAN_POINT ( 'NONE',  ( 1.530808498934191521E-15, 1.862499998088169129, -25.00000000000000000 ) ) ;
#10910 = ADVANCED_FACE ( 'NONE', ( #8752 ), #9528, .T. ) ;
#10911 = CARTESIAN_POINT ( 'NONE',  ( 0.5000000000000000000, 19.03096903053430822, 6.982120021884467675 ) ) ;
#10912 = CARTESIAN_POINT ( 'NONE',  ( 24.62111388750000174, 3.281249999044085097, -10.19839929293505776 ) ) ;
#10913 = CYLINDRICAL_SURFACE ( 'NONE', #4825, 25.00000000000000000 ) ;
#10914 = EDGE_LOOP ( 'NONE', ( #3730, #8704, #8874 ) ) ;
#10915 = ORIENTED_EDGE ( 'NONE', *, *, #3282, .F. ) ;
#10916 = ORIENTED_EDGE ( 'NONE', *, *, #7828, .T. ) ;
#10917 =( BOUNDED_CURVE ( )  B_SPLINE_CURVE ( 2, ( #3386, #924, #10142, #3507, #5947, #10196, #9303, #4294, #7657 ),
 .UNSPECIFIED., .F., .F. ) 
 B_SPLINE_CURVE_WITH_KNOTS ( ( 3, 2, 2, 2, 3 ),
 ( 0.3500000000000000333, 0.3750000000000000555, 0.4000000000000000222, 0.4249999999999999889, 0.4500000000000000111 ),
 .UNSPECIFIED. ) 
 CURVE ( )  GEOMETRIC_REPRESENTATION_ITEM ( )  RATIONAL_B_SPLINE_CURVE ( ( 0.9999999999999997780, 0.9238795325112869605, 1.000000000000000000, 0.9238795325112867385, 1.000000000000000000, 0.9238795325112867385, 1.000000000000000000, 0.9238795325112867385, 1.000000000000000000 ) ) 
 REPRESENTATION_ITEM ( '' )  );
#10918 = ADVANCED_FACE ( 'NONE', ( #5992 ), #300, .F. ) ;
#10919 = ORIENTED_EDGE ( 'NONE', *, *, #791, .T. ) ;
#10920 = ADVANCED_FACE ( 'NONE', ( #2765 ), #5448, .T. ) ;
#10921 = AXIS2_PLACEMENT_3D ( 'NONE', #1697, #6910, #10034 ) ;
#10922 = CARTESIAN_POINT ( 'NONE',  ( -1.500000000000001332, 0.000000000000000000, 0.000000000000000000 ) ) ;
#10923 = FACE_OUTER_BOUND ( 'NONE', #1134, .T. ) ;
#10924 = EDGE_CURVE ( 'NONE', #652, #93, #139, .T. ) ;
#10925 = CARTESIAN_POINT ( 'NONE',  ( 12.13990010960486288, 25.00000000000000000, -10.47307621135337108 ) ) ;
#10926 = LINE ( 'NONE', #7544, #1831 ) ;
#10927 = CARTESIAN_POINT ( 'NONE',  ( 23.22996358440884990, 5.000000000000000000, 8.988974415371478344 ) ) ;
#10928 = ADVANCED_FACE ( 'NONE', ( #188, #2024 ), #3548, .F. ) ;
#10929 = CARTESIAN_POINT ( 'NONE',  ( 3.716506350946109372, 19.74999999999999645, -5.437177826491055299 ) ) ;
#10930 = DIRECTION ( 'NONE',  ( 1.000000000000000000, 0.000000000000000000, 0.000000000000000000 ) ) ;
#10931 = CARTESIAN_POINT ( 'NONE',  ( 0.000000000000000000, 28.00000000000000000, 0.000000000000000000 ) ) ;
#10932 = DIRECTION ( 'NONE',  ( 0.000000000000000000, 0.000000000000000000, 1.000000000000000000 ) ) ;
#10933 = ORIENTED_EDGE ( 'NONE', *, *, #8153, .F. ) ;
#10934 = CARTESIAN_POINT ( 'NONE',  ( -9.875000000000143885, 25.00000000000000000, -17.10400172474258085 ) ) ;
#10935 = APPLICATION_PROTOCOL_DEFINITION ( 'draft international standard', 'automotive_design', 1998, #10061 ) ;
#10936 = ADVANCED_FACE ( 'NONE', ( #973 ), #8961, .T. ) ;
#10937 = DIRECTION ( 'NONE',  ( 0.000000000000000000, -2.775557561562888270E-17, -1.000000000000000000 ) ) ;
#10938 = ORIENTED_EDGE ( 'NONE', *, *, #5408, .T. ) ;
#10939 = VECTOR ( 'NONE', #4159, 1000.000000000000000 ) ;
#10940 = CYLINDRICAL_SURFACE ( 'NONE', #4117, 5.525000000000006573 ) ;
#10941 = CARTESIAN_POINT ( 'NONE',  ( -10.19839929293507375, 3.906249999044085097, 24.62111388749999108 ) ) ;
#10942 = ORIENTED_EDGE ( 'NONE', *, *, #9089, .T. ) ;
#10943 = AXIS2_PLACEMENT_3D ( 'NONE', #8675, #10337, #7137 ) ;
#10944 = CARTESIAN_POINT ( 'NONE',  ( 24.62111388749999463, 2.331249999044084031, 10.19839929293507730 ) ) ;
#10945 = EDGE_CURVE ( 'NONE', #1513, #1422, #2598, .T. ) ;
#10946 = CARTESIAN_POINT ( 'NONE',  ( 0.000000000000000000, 31.00000000000000000, -7.500000000000000888 ) ) ;
#10947 = NEXT_ASSEMBLY_USAGE_OCCURRENCE ( 'NAUO1', ' ', ' ', #8315, #3451, $ ) ;
#10948 = NEXT_ASSEMBLY_USAGE_OCCURRENCE ( 'NAUO2', ' ', ' ', #8315, #5432, $ ) ;
#10949 = NEXT_ASSEMBLY_USAGE_OCCURRENCE ( 'NAUO3', ' ', ' ', #8315, #6924, $ ) ;
#10950 = NEXT_ASSEMBLY_USAGE_OCCURRENCE ( 'NAUO4', ' ', ' ', #8315, #14, $ ) ;
#10951 = NEXT_ASSEMBLY_USAGE_OCCURRENCE ( 'NAUO5', ' ', ' ', #8315, #10146, $ ) ;
#10952 = NEXT_ASSEMBLY_USAGE_OCCURRENCE ( 'NAUO6', ' ', ' ', #8315, #4432, $ ) ;
#10953 = NEXT_ASSEMBLY_USAGE_OCCURRENCE ( 'NAUO7', ' ', ' ', #8315, #8124, $ ) ;
#10954 = NEXT_ASSEMBLY_USAGE_OCCURRENCE ( 'NAUO8', ' ', ' ', #8315, #7512, $ ) ;
ENDSEC;
END-ISO-10303-21;
